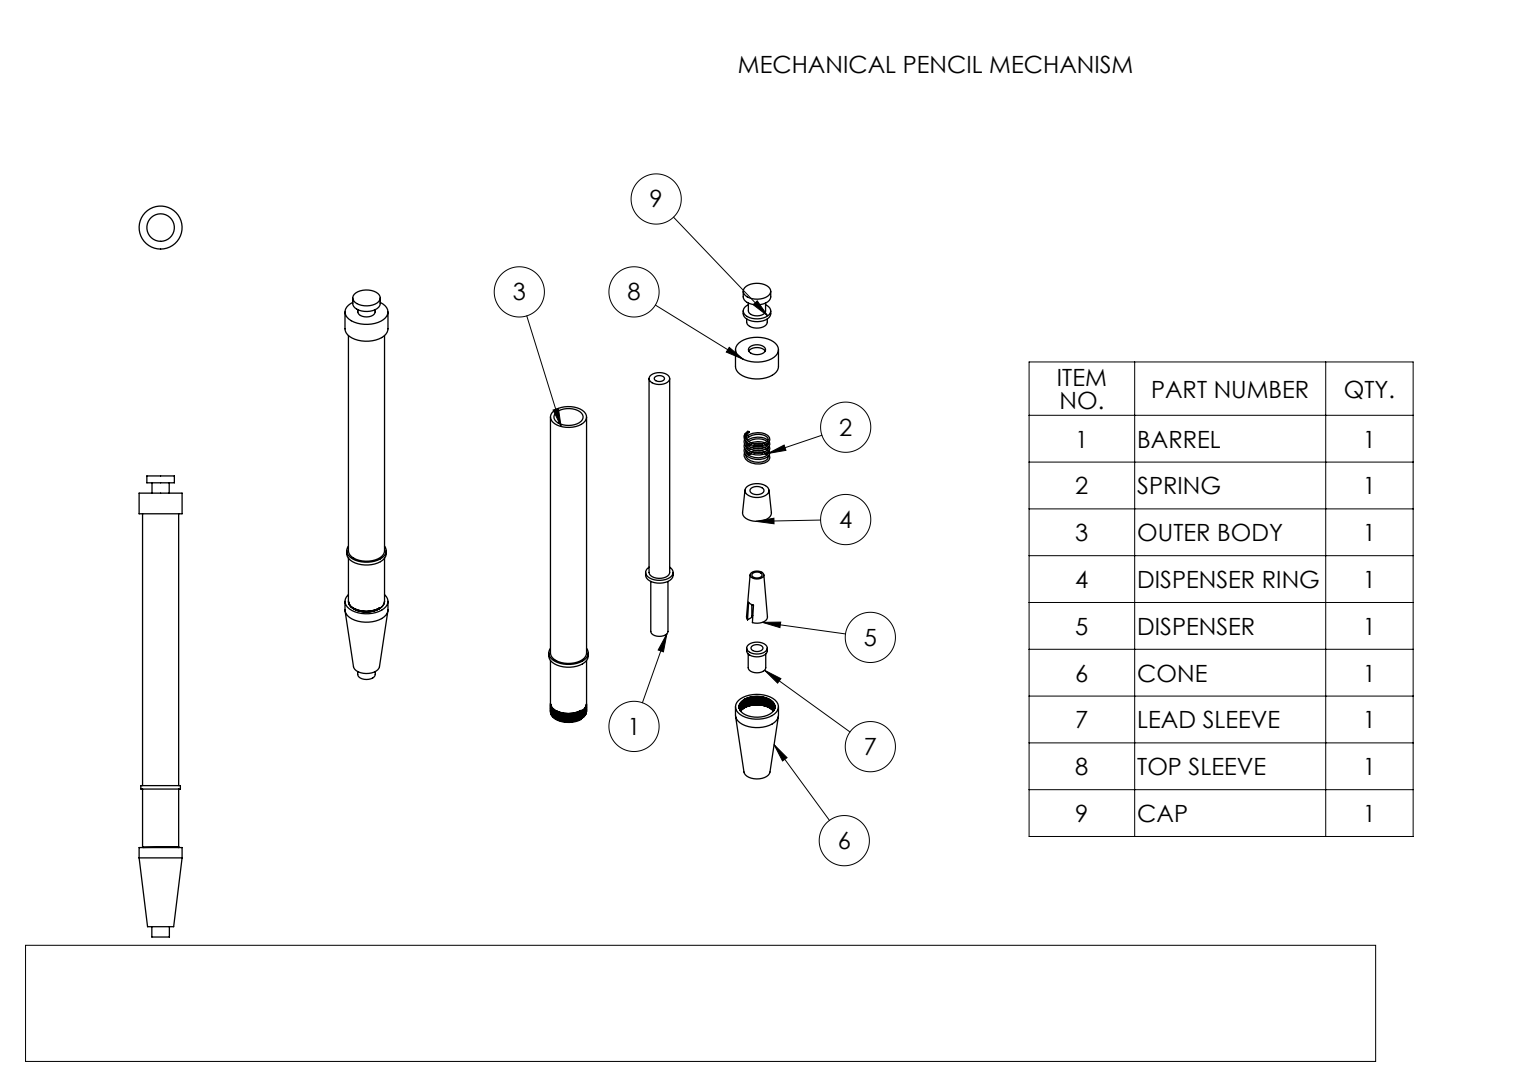
ISO-10303-21;
HEADER;
FILE_DESCRIPTION (('STEP AP214'),
    '1' );
FILE_NAME ('MAS-161',
    '2026-10-27T10:49:47',
    ( '' ),
    ( '' ),
    'SwSTEP 2.0',
    'SolidWorks 2026',
    '' );
FILE_SCHEMA (( 'AUTOMOTIVE_DESIGN' ));
ENDSEC;

DATA;
#1 = ORIENTED_EDGE ( 'NONE', *, *, #5722, .T. ) ;
#2 = FILL_AREA_STYLE ('',( #5004 ) ) ;
#3 = CARTESIAN_POINT ( 'NONE',  ( 1.113604000661152470E-15, -29.93749999999999645, 6.062177826491070398 ) ) ;
#4 = CARTESIAN_POINT ( 'NONE',  ( 5.114683531250000748, -27.33854166700806587, -2.952963913586932776 ) ) ;
#5 = CARTESIAN_POINT ( 'NONE',  ( -2.108492589042352261, -1.550659073900639395, 2.134148098076933397 ) ) ;
#6 = CARTESIAN_POINT ( 'NONE',  ( 5.250000000000000000, -29.22916666666666430, -3.031088913245534755 ) ) ;
#7 = CARTESIAN_POINT ( 'NONE',  ( 1.000000000000000000, -30.99987166532831395, 2.582963027349738816 ) ) ;
#8 = ADVANCED_FACE ( 'NONE', ( #6134 ), #1014, .T. ) ;
#9 = CARTESIAN_POINT ( 'NONE',  ( 5.114683531250000748, -28.90104166700806587, -2.952963913586932776 ) ) ;
#10 = VECTOR ( 'NONE', #8817, 1000.000000000000000 ) ;
#11 =( NAMED_UNIT ( * ) SI_UNIT ( $, .STERADIAN. ) SOLID_ANGLE_UNIT ( ) );
#12 = CARTESIAN_POINT ( 'NONE',  ( -5.114683531249999859, -28.31770833367473372, -2.952963913586935440 ) ) ;
#13 = CARTESIAN_POINT ( 'NONE',  ( 2.625000000000002220, -29.35416666598386826, 4.546633369868302132 ) ) ;
#14 = CARTESIAN_POINT ( 'NONE',  ( 5.249999999999999112, -27.54166666598387181, -3.031088913245536975 ) ) ;
#15 = CARTESIAN_POINT ( 'NONE',  ( -2.593667801677444817, -2.017599804162952387E-16, 2.576081167903025104 ) ) ;
#16 = DIRECTION ( 'NONE',  ( 1.000000000000000000, 0.000000000000000000, -0.000000000000000000 ) ) ;
#17 = CARTESIAN_POINT ( 'NONE',  ( -5.114683531249999859, -29.56770833367473017, -2.952963913586935440 ) ) ;
#18 = CARTESIAN_POINT ( 'NONE',  ( -1.467888652719046449, -6.949340926099361049, 3.492485675378536047 ) ) ;
#19 = EDGE_LOOP ( 'NONE', ( #3750, #4304, #1709, #1694 ) ) ;
#20 = CARTESIAN_POINT ( 'NONE',  ( -5.249999999999997335, -28.91666666598386826, 3.031088913245538308 ) ) ;
#21 = CARTESIAN_POINT ( 'NONE',  ( 2.557341765624996821, -29.15104166700806587, 4.429445870380401828 ) ) ;
#22 = EDGE_LOOP ( 'NONE', ( #1173, #7087 ) ) ;
#23 = ORIENTED_EDGE ( 'NONE', *, *, #2711, .F. ) ;
#24 = CARTESIAN_POINT ( 'NONE',  ( 0.000000000000000000, -53.00000000000000000, 0.000000000000000000 ) ) ;
#25 = CARTESIAN_POINT ( 'NONE',  ( 0.01814118441313990887, -6.550659073900639839, 3.500000000000000000 ) ) ;
#26 = CARTESIAN_POINT ( 'NONE',  ( 4.898587196589412829E-16, 81.00000000000001421, 4.000000000000000000 ) ) ;
#27 = VERTEX_POINT ( 'NONE', #2510 ) ;
#28 = PRODUCT_DEFINITION_SHAPE ( 'NONE', 'NONE',  #6653 ) ;
#29 = CARTESIAN_POINT ( 'NONE',  ( 6.429395695523604153E-16, -27.00000000000000000, 5.250000000000000000 ) ) ;
#30 = CARTESIAN_POINT ( 'NONE',  ( -1.000000000000000000, -29.00000000000000355, -1.118033988749894680 ) ) ;
#31 = CARTESIAN_POINT ( 'NONE',  ( 2.625000000000002220, -28.91666666666666785, 4.546633369868302132 ) ) ;
#32 = CARTESIAN_POINT ( 'NONE',  ( -5.114683531249999859, -28.75520833367473017, -2.952963913586935440 ) ) ;
#33 = CARTESIAN_POINT ( 'NONE',  ( 3.492485675378536047, -0.9493409260993610488, 1.467888652719046672 ) ) ;
#34 = CARTESIAN_POINT ( 'NONE',  ( -5.249999999999999112, -28.70833333265053611, -3.031088913245534755 ) ) ;
#35 = ADVANCED_FACE ( 'NONE', ( #4002 ), #1115, .T. ) ;
#36 = CARTESIAN_POINT ( 'NONE',  ( 1.260781871532495657, -2.949340926099361937, -2.992485675378538268 ) ) ;
#37 =( BOUNDED_CURVE ( )  B_SPLINE_CURVE ( 2, ( #980, #8007, #3923, #3739, #4569, #5213, #3046, #6700, #6561 ),
 .UNSPECIFIED., .F., .F. ) 
 B_SPLINE_CURVE_WITH_KNOTS ( ( 3, 2, 2, 2, 3 ),
 ( 0.1041666666666666713, 0.1111111111111111049, 0.1250000000000000000, 0.1388888888888888951, 0.1458333333333333426 ),
 .UNSPECIFIED. ) 
 CURVE ( )  GEOMETRIC_REPRESENTATION_ITEM ( )  RATIONAL_B_SPLINE_CURVE ( ( 0.9330127018922194093, 0.9330127018922194093, 1.000000000000000000, 0.8660254037844387076, 1.000000000000000000, 0.8660254037844387076, 1.000000000000000000, 0.9330127018922194093, 0.9330127018922194093 ) ) 
 REPRESENTATION_ITEM ( '' )  );
#38 = CARTESIAN_POINT ( 'NONE',  ( 1.406733260263403507, -28.57366454968462577, -5.249999999999994671 ) ) ;
#39 = CARTESIAN_POINT ( 'NONE',  ( 5.385316468750000141, -27.73437499965860198, -6.595110575850215044E-16 ) ) ;
#40 = CARTESIAN_POINT ( 'NONE',  ( 1.638713065079247855, -2.450659073900638862, -4.007514324621431534 ) ) ;
#41 = VECTOR ( 'NONE', #4397, 1000.000000000000000 ) ;
#42 = SURFACE_STYLE_FILL_AREA ( #6405 ) ;
#43 = APPLICATION_CONTEXT ( 'automotive_design' ) ;
#44 = CARTESIAN_POINT ( 'NONE',  ( 2.033577675846918216E-14, -27.81249999999999645, 5.250000000000000888 ) ) ;
#45 = ORIENTED_EDGE ( 'NONE', *, *, #6013, .T. ) ;
#46 = CARTESIAN_POINT ( 'NONE',  ( 5.385316468750000141, -27.45312499965860198, -6.595110575850215044E-16 ) ) ;
#47 =( GEOMETRIC_REPRESENTATION_CONTEXT ( 3 ) GLOBAL_UNCERTAINTY_ASSIGNED_CONTEXT ( ( #2399 ) ) GLOBAL_UNIT_ASSIGNED_CONTEXT ( ( #4022, #5674, #2943 ) ) REPRESENTATION_CONTEXT ( 'NONE', 'WORKASPACE' ) );
#48 = ORIENTED_EDGE ( 'NONE', *, *, #6878, .T. ) ;
#49 = CARTESIAN_POINT ( 'NONE',  ( -5.385316468750000141, -27.32812499965860198, 0.000000000000000000 ) ) ;
#50 = CARTESIAN_POINT ( 'NONE',  ( 2.992485675378565357, -0.6506590739006395951, -1.260781871532430376 ) ) ;
#51 = ORIENTED_EDGE ( 'NONE', *, *, #9169, .T. ) ;
#52 = CARTESIAN_POINT ( 'NONE',  ( -2.624999999999998668, -28.91666666666666785, -4.546633369868303021 ) ) ;
#53 = CYLINDRICAL_SURFACE ( 'NONE', #3617, 5.250000000000000000 ) ;
#54 = CIRCLE ( 'NONE', #4368, 3.000000000000000444 ) ;
#55 = CARTESIAN_POINT ( 'NONE',  ( 5.114683531250000748, -28.42187500034139802, 0.000000000000000000 ) ) ;
#56 = CARTESIAN_POINT ( 'NONE',  ( 3.616337804771879580E-16, -28.35937500034139447, -5.905927827173866440 ) ) ;
#57 = DIRECTION ( 'NONE',  ( 0.000000000000000000, 0.000000000000000000, -1.000000000000000000 ) ) ;
#58 = CARTESIAN_POINT ( 'NONE',  ( 2.324088772396477476E-15, -27.49999999931720751, -5.250000000000000000 ) ) ;
#59 = CARTESIAN_POINT ( 'NONE',  ( -2.110065146580993645, -1.191525181865938352E-11, 2.889420178070662093 ) ) ;
#60 = LINE ( 'NONE', #4208, #5677 ) ;
#61 = CARTESIAN_POINT ( 'NONE',  ( -1.431606283892620235, -7.949340926099361049, -3.507514324621463953 ) ) ;
#62 = CARTESIAN_POINT ( 'NONE',  ( -1.467888652719046449, -3.749340926099360871, 3.492485675378536047 ) ) ;
#63 = EDGE_LOOP ( 'NONE', ( #2688, #9138, #7959, #2580 ) ) ;
#64 = CARTESIAN_POINT ( 'NONE',  ( 2.161402558328724325E-14, -28.99999999931720751, -5.250000000000000000 ) ) ;
#65 = CARTESIAN_POINT ( 'NONE',  ( 5.250000000000000000, -27.03125000068279604, 0.000000000000000000 ) ) ;
#66 = EDGE_LOOP ( 'NONE', ( #5126, #5183, #1901, #2100 ) ) ;
#67 = ORIENTED_EDGE ( 'NONE', *, *, #7886, .F. ) ;
#68 = DIRECTION ( 'NONE',  ( 0.000000000000000000, -1.000000000000000000, 0.000000000000000000 ) ) ;
#69 = CARTESIAN_POINT ( 'NONE',  ( 2.487701488670203354, -6.750659073900639129, 2.462045979635629323 ) ) ;
#70 = CARTESIAN_POINT ( 'NONE',  ( 1.000000000000000000, -29.00000000000000355, -2.431755684948965435 ) ) ;
#71 = EDGE_LOOP ( 'NONE', ( #3557, #48, #247, #244 ) ) ;
#72 = DIRECTION ( 'NONE',  ( -0.000000000000000000, 1.000000000000000000, -0.000000000000000000 ) ) ;
#73 = CYLINDRICAL_SURFACE ( 'NONE', #5825, 2.499999999999999556 ) ;
#74 = EDGE_CURVE ( 'NONE', #2716, #8116, #2372, .T. ) ;
#75 = LINE ( 'NONE', #5700, #8771 ) ;
#76 = CARTESIAN_POINT ( 'NONE',  ( -2.557341765624999042, -27.02604166700806232, -4.429445870380400052 ) ) ;
#77 = CARTESIAN_POINT ( 'NONE',  ( -3.507514324621464397, -0.3493409260993610710, 1.431606283892619347 ) ) ;
#78 = CARTESIAN_POINT ( 'NONE',  ( -3.000000000000000444, -5.049340926099361582, -0.01814118441320822922 ) ) ;
#79 = EDGE_CURVE ( 'NONE', #7374, #1200, #6541, .T. ) ;
#80 = DIRECTION ( 'NONE',  ( 0.000000000000000000, 0.000000000000000000, -1.000000000000000000 ) ) ;
#81 = CARTESIAN_POINT ( 'NONE',  ( -3.807688866302469071E-16, -28.17187499965860553, -6.218427825808274356 ) ) ;
#82 = CARTESIAN_POINT ( 'NONE',  ( 0.01814118441321938349, -1.449340926099360827, -4.000000000000000000 ) ) ;
#83 = FACE_OUTER_BOUND ( 'NONE', #879, .T. ) ;
#84 = CARTESIAN_POINT ( 'NONE',  ( 0.000000000000000000, -30.00000000000000000, 0.000000000000000000 ) ) ;
#85 =( BOUNDED_CURVE ( )  B_SPLINE_CURVE ( 2, ( #9078, #8390, #6906, #2534, #530 ),
 .UNSPECIFIED., .F., .F. ) 
 B_SPLINE_CURVE_WITH_KNOTS ( ( 3, 2, 3 ),
 ( 0.9791666666666667407, 0.9861111111111111605, 1.000000000000000000 ),
 .UNSPECIFIED. ) 
 CURVE ( )  GEOMETRIC_REPRESENTATION_ITEM ( )  RATIONAL_B_SPLINE_CURVE ( ( 0.9330127018922192983, 0.9330127018922198534, 1.000000000000000000, 0.8660254037844387076, 1.000000000000000000 ) ) 
 REPRESENTATION_ITEM ( '' )  );
#86 = ORIENTED_EDGE ( 'NONE', *, *, #5112, .F. ) ;
#87 = CARTESIAN_POINT ( 'NONE',  ( -5.250000000000000000, -29.75000000000000000, 0.000000000000000000 ) ) ;
#88 = EDGE_LOOP ( 'NONE', ( #8020, #7590 ) ) ;
#89 = LINE ( 'NONE', #7305, #4201 ) ;
#90 = CARTESIAN_POINT ( 'NONE',  ( 2.134148098076933397, -5.150659073900639484, 2.108492589042352261 ) ) ;
#91 = ORIENTED_EDGE ( 'NONE', *, *, #709, .F. ) ;
#92 = CARTESIAN_POINT ( 'NONE',  ( -2.625000000000002220, -28.58333333333333215, 4.546633369868302132 ) ) ;
#93 = CYLINDRICAL_SURFACE ( 'NONE', #1391, 5.250000000000000000 ) ;
#94 = CARTESIAN_POINT ( 'NONE',  ( -5.114683531250000748, -28.06770833367473017, -2.952963913586935440 ) ) ;
#95 =( NAMED_UNIT ( * ) SI_UNIT ( $, .STERADIAN. ) SOLID_ANGLE_UNIT ( ) );
#96 = CARTESIAN_POINT ( 'NONE',  ( 5.114683531249998971, -27.44270833367473017, 2.952963913586936329 ) ) ;
#97 = EDGE_CURVE ( 'NONE', #451, #2823, #2727, .T. ) ;
#98 = CARTESIAN_POINT ( 'NONE',  ( 2.161402558328724325E-14, -28.74999999931720751, -5.250000000000000000 ) ) ;
#99 = PRODUCT_DEFINITION_SHAPE ( 'NONE', 'NONE',  #1543 ) ;
#100 = CARTESIAN_POINT ( 'NONE',  ( 0.000000000000000000, -30.00000000000000000, 4.250000000000000000 ) ) ;
#101 = DIRECTION ( 'NONE',  ( 0.000000000000000000, 1.000000000000000000, 0.000000000000000000 ) ) ;
#102 = CARTESIAN_POINT ( 'NONE',  ( -5.250000000000000888, -27.38541666734946389, 3.031088913245533423 ) ) ;
#103 = CARTESIAN_POINT ( 'NONE',  ( 3.616337804771879580E-16, -29.60937500034139447, -5.905927827173866440 ) ) ;
#104 = CARTESIAN_POINT ( 'NONE',  ( 3.492485675378536047, -7.349340926099362292, 1.467888652719046672 ) ) ;
#105 = VERTEX_POINT ( 'NONE', #315 ) ;
#106 = CARTESIAN_POINT ( 'NONE',  ( -6.972266317189433020E-16, -27.06250000000000000, -5.250000000000000000 ) ) ;
#107 = CARTESIAN_POINT ( 'NONE',  ( 0.000000000000000000, -29.00000000000000355, -1.499999999999999778 ) ) ;
#108 = CARTESIAN_POINT ( 'NONE',  ( -2.557341765624999042, -28.27604166700806587, -4.429445870380400052 ) ) ;
#109 = EDGE_LOOP ( 'NONE', ( #5447, #4357, #2145, #3993 ) ) ;
#110 =( BOUNDED_CURVE ( )  B_SPLINE_CURVE ( 2, ( #4913, #7058, #9104, #4136, #4827, #6270, #4182, #2042, #682 ),
 .UNSPECIFIED., .F., .T. ) 
 B_SPLINE_CURVE_WITH_KNOTS ( ( 3, 2, 2, 2, 3 ),
 ( 0.3541666666666666852, 0.3611111111111111049, 0.3750000000000000000, 0.3888888888888888951, 0.3958333333333333703 ),
 .UNSPECIFIED. ) 
 CURVE ( )  GEOMETRIC_REPRESENTATION_ITEM ( )  RATIONAL_B_SPLINE_CURVE ( ( 0.9330127018922194093, 0.9330127018922196314, 1.000000000000000000, 0.8660254037844387076, 1.000000000000000000, 0.8660254037844387076, 1.000000000000000000, 0.9330127018922190762, 0.9330127018922194093 ) ) 
 REPRESENTATION_ITEM ( '' )  );
#111 = ORIENTED_EDGE ( 'NONE', *, *, #9064, .F. ) ;
#112 = CARTESIAN_POINT ( 'NONE',  ( -2.033577675846918216E-14, -29.68750000000000355, 5.250000000000000888 ) ) ;
#113 = CARTESIAN_POINT ( 'NONE',  ( -5.385316468750001029, -27.13020833299193413, -3.109213912904136734 ) ) ;
#114 = CARTESIAN_POINT ( 'NONE',  ( -4.000000000000000000, -7.750659073900639129, 0.01814118441313491634 ) ) ;
#115 = CARTESIAN_POINT ( 'NONE',  ( 1.836970198721029688E-16, -29.00000000000000355, 1.499999999999999778 ) ) ;
#116 = VERTEX_POINT ( 'NONE', #4866 ) ;
#117 = DIRECTION ( 'NONE',  ( 0.000000000000000000, -0.000000000000000000, 1.000000000000000000 ) ) ;
#118 = CARTESIAN_POINT ( 'NONE',  ( 5.250000000000000000, -29.03125000068279604, 0.000000000000000000 ) ) ;
#119 = CARTESIAN_POINT ( 'NONE',  ( -2.033577675846918216E-14, -29.87499999931720396, 5.250000000000000888 ) ) ;
#120 = UNCERTAINTY_MEASURE_WITH_UNIT (LENGTH_MEASURE( 1.000000000000000082E-05 ), #327, 'distance_accuracy_value', 'NONE');
#121 = CARTESIAN_POINT ( 'NONE',  ( 2.557341765624996821, -27.15104166700806587, 4.429445870380401828 ) ) ;
#122 = CARTESIAN_POINT ( 'NONE',  ( -2.487701488670255312, -2.049340926099361582, 2.462045979635577808 ) ) ;
#123 = CIRCLE ( 'NONE', #1315, 2.629341307491595447 ) ;
#124 = CYLINDRICAL_SURFACE ( 'NONE', #4810, 5.250000000000000000 ) ;
#125 = CARTESIAN_POINT ( 'NONE',  ( 3.000000000000000444, -5.849340926099360516, 0.01814118441320859698 ) ) ;
#126 = LINE ( 'NONE', #643, #8886 ) ;
#127 = CARTESIAN_POINT ( 'NONE',  ( -1.674995433905599462, -0.5493409260993608045, 3.992485675378533383 ) ) ;
#128 = DIRECTION ( 'NONE',  ( 0.000000000000000000, 0.000000000000000000, 1.000000000000000000 ) ) ;
#129 = AXIS2_PLACEMENT_3D ( 'NONE', #454, #8273, #5425 ) ;
#130 = CARTESIAN_POINT ( 'NONE',  ( 0.000000000000000000, -9.999999999999998224, 0.000000000000000000 ) ) ;
#131 = ADVANCED_FACE ( 'NONE', ( #1342 ), #6353, .T. ) ;
#132 = ORIENTED_EDGE ( 'NONE', *, *, #6059, .F. ) ;
#133 = CARTESIAN_POINT ( 'NONE',  ( -5.385316468750000141, -28.82812499965860198, 0.000000000000000000 ) ) ;
#134 = FACE_OUTER_BOUND ( 'NONE', #6393, .T. ) ;
#135 = ORIENTED_EDGE ( 'NONE', *, *, #4743, .T. ) ;
#136 = AXIS2_PLACEMENT_3D ( 'NONE', #8169, #1046, #2544 ) ;
#137 = CARTESIAN_POINT ( 'NONE',  ( -2.692658234375000514, -27.61979166632526628, -4.663820869356205989 ) ) ;
#138 = CARTESIAN_POINT ( 'NONE',  ( 3.007514324621436863, -6.850659073900641438, 1.224499502706140719 ) ) ;
#139 = ORIENTED_EDGE ( 'NONE', *, *, #8501, .F. ) ;
#140 = CARTESIAN_POINT ( 'NONE',  ( 2.624999999999996891, -29.04166666666666785, 4.546633369868304797 ) ) ;
#141 = CARTESIAN_POINT ( 'NONE',  ( 2.624999999999996891, -29.79166666666666430, 4.546633369868304797 ) ) ;
#142 = PRESENTATION_LAYER_ASSIGNMENT (  '', '', ( #446 ) ) ;
#143 = CARTESIAN_POINT ( 'NONE',  ( 5.114683531250000748, -27.67187500034139802, 0.000000000000000000 ) ) ;
#144 = EDGE_CURVE ( 'NONE', #7348, #2527, #110, .T. ) ;
#145 =( LENGTH_UNIT ( ) NAMED_UNIT ( * ) SI_UNIT ( .MILLI., .METRE. ) );
#146 = CARTESIAN_POINT ( 'NONE',  ( 3.616337804771879580E-16, -27.35937500034140157, -5.905927827173866440 ) ) ;
#147 = AXIS2_PLACEMENT_3D ( 'NONE', #204, #847, #6661 ) ;
#148 = DIRECTION ( 'NONE',  ( 0.000000000000000000, 0.000000000000000000, 1.000000000000000000 ) ) ;
#149 = CARTESIAN_POINT ( 'NONE',  ( 1.431606283892619125, -5.549340926099361582, 3.507514324621464397 ) ) ;
#150 = FACE_OUTER_BOUND ( 'NONE', #5421, .T. ) ;
#151 = DIRECTION ( 'NONE',  ( 0.000000000000000000, -1.000000000000000000, 0.000000000000000000 ) ) ;
#152 = CARTESIAN_POINT ( 'NONE',  ( -1.467888652719046449, -6.949340926099361049, 3.492485675378536047 ) ) ;
#153 = DIRECTION ( 'NONE',  ( 1.000000000000000000, 0.000000000000000000, 0.000000000000000000 ) ) ;
#154 = VERTEX_POINT ( 'NONE', #6883 ) ;
#155 = CARTESIAN_POINT ( 'NONE',  ( 2.487701488670203354, -6.750659073900639129, 2.462045979635629323 ) ) ;
#156 = AXIS2_PLACEMENT_3D ( 'NONE', #2203, #2343, #5173 ) ;
#157 = CARTESIAN_POINT ( 'NONE',  ( 2.557341765624996821, -28.65104166700806587, 4.429445870380401828 ) ) ;
#158 = ORIENTED_EDGE ( 'NONE', *, *, #8454, .T. ) ;
#159 = DIRECTION ( 'NONE',  ( 0.000000000000000000, 0.000000000000000000, 1.000000000000000000 ) ) ;
#160 = CARTESIAN_POINT ( 'NONE',  ( 1.975475456537005874E-15, -29.62499999931719685, 5.249999999999999112 ) ) ;
#161 = CARTESIAN_POINT ( 'NONE',  ( -1.674995433905516196, -5.850659073900638774, -3.992485675378566690 ) ) ;
#162 = SURFACE_STYLE_USAGE ( .BOTH. , #5228 ) ;
#163 = ORIENTED_EDGE ( 'NONE', *, *, #1050, .T. ) ;
#164 = CARTESIAN_POINT ( 'NONE',  ( -2.625000000000000444, -27.97916666598386826, -4.546633369868303021 ) ) ;
#165 = CARTESIAN_POINT ( 'NONE',  ( 5.250000000000000000, -29.89062500034139802, 0.000000000000000000 ) ) ;
#166 =( BOUNDED_SURFACE ( )  B_SPLINE_SURFACE ( 1, 2, ( 
 ( #818, #6351, #7897, #2127, #6396, #4313, #4951, #7148, #3203, #6718, #3899, #5281, #6630, #911, #4591, #7235, #8126, #4545, #1608, #8029, #1563, #6587, #3708, #352, #8774, #6533, #1660, #1756, #258, #958, #3109, #3758, #6675, #8725, #7332, #4500, #215, #859, #1053, #7285, #3067, #3804, #3016, #5234, #5886, #5091, #4447, #167, #2357, #7377, #305, #5186, #5841, #6023, #5933, #2404, #8079, #8680, #1707, #1003, #7942, #3849, #2312, #3158, #5976, #8819, #2455, #2263, #5138, #7428, #4404, #7981, #4124, #8269, #545, #7618, #1856, #6123, #7569, #1243, #4085, #4819, #1104, #6920, #1900, #6958, #1989, #4775, #589, #3433, #1946, #3386, #1149, #4683, #3246, #6823, #6218, #8223, #2553, #7663, #8860, #9047, #5420, #6173, #4636, #5373, #7474, #7520, #2500, #399, #2692, #8952, #6772, #3992, #5323, #5519, #8364, #1285, #6070, #8177, #449, #1803, #3295, #6873, #3944, #4728, #1198, #499, #2603, #4041, #8906, #3344, #9000, #2647, #5469, #8315, #2033, #1328, #7703, #4856, #8406, #9093, #5561, #7005, #630 ),
 ( #2737, #6262, #4171, #7436, #8826, #964, #4457, #8135, #1571, #2461, #8086, #5147, #2366, #5099, #918, #7244, #1061, #3117, #868, #5196, #5286, #3811, #4510, #6636, #7294, #1010, #3073, #1667, #8038, #3905, #1713, #4552, #3768, #1618, #175, #6595, #7386, #7989, #8688, #1763, #6728, #3164, #7339, #5940, #4413, #2319, #3718, #225, #359, #6543, #3858, #5894, #3027, #8734, #2272, #4598, #5802, #8640, #5849, #6681, #265, #7949, #8782, #2411, #5242, #311, #5985, #6950, #6995, #2773, #3551, #4115, #2023, #5510, #3463, #579, #8353, #621, #750, #2861, #2724, #703, #4808, #4933, #3423, #5679, #6373, #1978, #4848, #6209, #7694, #4247, #7790, #7127, #5637, #6331, #2063, #2107, #8526, #2680, #9084, #8397, #9038, #6252, #13, #5593, #2816, #7654, #5551, #1277, #7039, #1318, #4891, #1408, #8486, #7743, #4162, #6292, #9128, #1447, #4291, #8437, #9167, #7081, #2155, #664, #1365, #4204, #3508, #4974, #7828, #5912, #4337, #7263, #4428, #797, #1687, #1544, #3641, #4527, #2335, #7172, #5215, #839, #7357 ) ),
 .UNSPECIFIED., .F., .F., .T. ) 
 B_SPLINE_SURFACE_WITH_KNOTS ( ( 2, 2 ),
 ( 3, 2, 2, 2, 2, 2, 2, 2, 2, 2, 2, 2, 2, 2, 2, 2, 2, 2, 2, 2, 2, 2, 2, 2, 2, 2, 2, 2, 2, 2, 2, 2, 2, 2, 2, 2, 2, 2, 2, 2, 2, 2, 2, 2, 2, 2, 2, 2, 2, 2, 2, 2, 2, 2, 2, 2, 2, 2, 2, 2, 2, 2, 2, 2, 2, 2, 2, 2, 2, 2, 2, 2, 3 ),
 ( 0.000000000000000000, 1.000000000000000000 ),
 ( 0.000000000000000000, 0.01388888888888888812, 0.02777777777777777624, 0.04166666666666666435, 0.05555555555555555247, 0.06944444444444444753, 0.08333333333333332871, 0.09722222222222222376, 0.1111111111111111049, 0.1250000000000000000, 0.1388888888888888951, 0.1527777777777777901, 0.1666666666666666574, 0.1805555555555555525, 0.1944444444444444475, 0.2083333333333333426, 0.2222222222222222099, 0.2361111111111111049, 0.2500000000000000000, 0.2638888888888888951, 0.2777777777777777901, 0.2916666666666666852, 0.3055555555555555802, 0.3194444444444444198, 0.3333333333333333148, 0.3472222222222222099, 0.3611111111111111049, 0.3750000000000000000, 0.3888888888888888951, 0.4027777777777777901, 0.4166666666666666852, 0.4305555555555555802, 0.4444444444444444198, 0.4583333333333333148, 0.4722222222222222099, 0.4861111111111111049, 0.5000000000000000000, 0.5138888888888888395, 0.5277777777777777901, 0.5416666666666666297, 0.5555555555555555802, 0.5694444444444444198, 0.5833333333333333703, 0.5972222222222222099, 0.6111111111111111605, 0.6250000000000000000, 0.6388888888888888395, 0.6527777777777777901, 0.6666666666666666297, 0.6805555555555555802, 0.6944444444444444198, 0.7083333333333333703, 0.7222222222222222099, 0.7361111111111111605, 0.7500000000000000000, 0.7638888888888888395, 0.7777777777777777901, 0.7916666666666666297, 0.8055555555555555802, 0.8194444444444444198, 0.8333333333333333703, 0.8472222222222222099, 0.8611111111111111605, 0.8750000000000000000, 0.8888888888888888395, 0.9027777777777777901, 0.9166666666666666297, 0.9305555555555555802, 0.9444444444444444198, 0.9583333333333333703, 0.9722222222222222099, 0.9861111111111111605, 1.000000000000000000 ),
 .UNSPECIFIED. ) 
 GEOMETRIC_REPRESENTATION_ITEM ( )  RATIONAL_B_SPLINE_SURFACE ( (
 ( 1.000000000000000000, 0.8660254037844387076, 1.000000000000000000, 0.8660254037844387076, 1.000000000000000000, 0.8660254037844387076, 1.000000000000000000, 0.8660254037844387076, 1.000000000000000000, 0.8660254037844387076, 1.000000000000000000, 0.8660254037844387076, 1.000000000000000000, 0.8660254037844387076, 1.000000000000000000, 0.8660254037844387076, 1.000000000000000000, 0.8660254037844387076, 1.000000000000000000, 0.8660254037844387076, 1.000000000000000000, 0.8660254037844387076, 1.000000000000000000, 0.8660254037844387076, 1.000000000000000000, 0.8660254037844387076, 1.000000000000000000, 0.8660254037844387076, 1.000000000000000000, 0.8660254037844387076, 1.000000000000000000, 0.8660254037844387076, 1.000000000000000000, 0.8660254037844387076, 1.000000000000000000, 0.8660254037844387076, 1.000000000000000000, 0.8660254037844387076, 1.000000000000000000, 0.8660254037844387076, 1.000000000000000000, 0.8660254037844387076, 1.000000000000000000, 0.8660254037844387076, 1.000000000000000000, 0.8660254037844387076, 1.000000000000000000, 0.8660254037844387076, 1.000000000000000000, 0.8660254037844387076, 1.000000000000000000, 0.8660254037844387076, 1.000000000000000000, 0.8660254037844387076, 1.000000000000000000, 0.8660254037844387076, 1.000000000000000000, 0.8660254037844387076, 1.000000000000000000, 0.8660254037844387076, 1.000000000000000000, 0.8660254037844387076, 1.000000000000000000, 0.8660254037844387076, 1.000000000000000000, 0.8660254037844387076, 1.000000000000000000, 0.8660254037844387076, 1.000000000000000000, 0.8660254037844387076, 1.000000000000000000, 0.8660254037844387076, 1.000000000000000000, 0.8660254037844387076, 1.000000000000000000, 0.8660254037844387076, 1.000000000000000000, 0.8660254037844387076, 1.000000000000000000, 0.8660254037844387076, 1.000000000000000000, 0.8660254037844387076, 1.000000000000000000, 0.8660254037844387076, 1.000000000000000000, 0.8660254037844387076, 1.000000000000000000, 0.8660254037844387076, 1.000000000000000000, 0.8660254037844387076, 1.000000000000000000, 0.8660254037844387076, 1.000000000000000000, 0.8660254037844387076, 1.000000000000000000, 0.8660254037844387076, 1.000000000000000000, 0.8660254037844387076, 1.000000000000000000, 0.8660254037844387076, 1.000000000000000000, 0.8660254037844387076, 1.000000000000000000, 0.8660254037844387076, 1.000000000000000000, 0.8660254037844387076, 1.000000000000000000, 0.8660254037844387076, 1.000000000000000000, 0.8660254037844387076, 1.000000000000000000, 0.8660254037844387076, 1.000000000000000000, 0.8660254037844387076, 1.000000000000000000, 0.8660254037844387076, 1.000000000000000000, 0.8660254037844387076, 1.000000000000000000, 0.8660254037844387076, 1.000000000000000000, 0.8660254037844387076, 1.000000000000000000, 0.8660254037844387076, 1.000000000000000000, 0.8660254037844387076, 1.000000000000000000, 0.8660254037844387076, 1.000000000000000000, 0.8660254037844387076, 1.000000000000000000, 0.8660254037844387076, 1.000000000000000000, 0.8660254037844387076, 1.000000000000000000, 0.8660254037844387076, 1.000000000000000000, 0.8660254037844387076, 1.000000000000000000, 0.8660254037844387076, 1.000000000000000000, 0.8660254037844387076, 1.000000000000000000, 0.8660254037844387076, 1.000000000000000000),
 ( 1.000000000000000000, 0.8660254037844387076, 1.000000000000000000, 0.8660254037844387076, 1.000000000000000000, 0.8660254037844387076, 1.000000000000000000, 0.8660254037844387076, 1.000000000000000000, 0.8660254037844387076, 1.000000000000000000, 0.8660254037844387076, 1.000000000000000000, 0.8660254037844387076, 1.000000000000000000, 0.8660254037844387076, 1.000000000000000000, 0.8660254037844387076, 1.000000000000000000, 0.8660254037844387076, 1.000000000000000000, 0.8660254037844387076, 1.000000000000000000, 0.8660254037844387076, 1.000000000000000000, 0.8660254037844387076, 1.000000000000000000, 0.8660254037844387076, 1.000000000000000000, 0.8660254037844387076, 1.000000000000000000, 0.8660254037844387076, 1.000000000000000000, 0.8660254037844387076, 1.000000000000000000, 0.8660254037844387076, 1.000000000000000000, 0.8660254037844387076, 1.000000000000000000, 0.8660254037844387076, 1.000000000000000000, 0.8660254037844387076, 1.000000000000000000, 0.8660254037844387076, 1.000000000000000000, 0.8660254037844387076, 1.000000000000000000, 0.8660254037844387076, 1.000000000000000000, 0.8660254037844387076, 1.000000000000000000, 0.8660254037844387076, 1.000000000000000000, 0.8660254037844387076, 1.000000000000000000, 0.8660254037844387076, 1.000000000000000000, 0.8660254037844387076, 1.000000000000000000, 0.8660254037844387076, 1.000000000000000000, 0.8660254037844387076, 1.000000000000000000, 0.8660254037844387076, 1.000000000000000000, 0.8660254037844387076, 1.000000000000000000, 0.8660254037844387076, 1.000000000000000000, 0.8660254037844387076, 1.000000000000000000, 0.8660254037844387076, 1.000000000000000000, 0.8660254037844387076, 1.000000000000000000, 0.8660254037844387076, 1.000000000000000000, 0.8660254037844387076, 1.000000000000000000, 0.8660254037844387076, 1.000000000000000000, 0.8660254037844387076, 1.000000000000000000, 0.8660254037844387076, 1.000000000000000000, 0.8660254037844387076, 1.000000000000000000, 0.8660254037844387076, 1.000000000000000000, 0.8660254037844387076, 1.000000000000000000, 0.8660254037844387076, 1.000000000000000000, 0.8660254037844387076, 1.000000000000000000, 0.8660254037844387076, 1.000000000000000000, 0.8660254037844387076, 1.000000000000000000, 0.8660254037844387076, 1.000000000000000000, 0.8660254037844387076, 1.000000000000000000, 0.8660254037844387076, 1.000000000000000000, 0.8660254037844387076, 1.000000000000000000, 0.8660254037844387076, 1.000000000000000000, 0.8660254037844387076, 1.000000000000000000, 0.8660254037844387076, 1.000000000000000000, 0.8660254037844387076, 1.000000000000000000, 0.8660254037844387076, 1.000000000000000000, 0.8660254037844387076, 1.000000000000000000, 0.8660254037844387076, 1.000000000000000000, 0.8660254037844387076, 1.000000000000000000, 0.8660254037844387076, 1.000000000000000000, 0.8660254037844387076, 1.000000000000000000, 0.8660254037844387076, 1.000000000000000000, 0.8660254037844387076, 1.000000000000000000, 0.8660254037844387076, 1.000000000000000000, 0.8660254037844387076, 1.000000000000000000, 0.8660254037844387076, 1.000000000000000000, 0.8660254037844387076, 1.000000000000000000, 0.8660254037844387076, 1.000000000000000000, 0.8660254037844387076, 1.000000000000000000, 0.8660254037844387076, 1.000000000000000000) ) ) 
 REPRESENTATION_ITEM ( '' )  SURFACE ( )  );
#167 = CARTESIAN_POINT ( 'NONE',  ( -5.385316468749998364, -28.08854166632526628, 3.109213912904140287 ) ) ;
#168 = CARTESIAN_POINT ( 'NONE',  ( 2.557341765625000818, -27.56770833367473017, -4.429445870380400052 ) ) ;
#169 = CARTESIAN_POINT ( 'NONE',  ( 2.462045979635577364, -2.449340926099361049, 2.487701488670255312 ) ) ;
#170 = CARTESIAN_POINT ( 'NONE',  ( 1.142306659890740623E-15, -27.26562499965860553, 6.218427825808274356 ) ) ;
#171 = CARTESIAN_POINT ( 'NONE',  ( 1.224499502706142273, -2.450659073900639751, -3.007514324621435531 ) ) ;
#172 = CARTESIAN_POINT ( 'NONE',  ( -5.249999999999997335, -29.41666666598387181, 3.031088913245538308 ) ) ;
#173 = EDGE_CURVE ( 'NONE', #105, #7348, #3624, .T. ) ;
#174 = CARTESIAN_POINT ( 'NONE',  ( -2.815599370228846876, -1.649340926099360560, -2.841254879263533262 ) ) ;
#175 = CARTESIAN_POINT ( 'NONE',  ( -2.624999999999996891, -27.89583333265053255, 4.546633369868304797 ) ) ;
#176 = LINE ( 'NONE', #7340, #7480 ) ;
#177 = CARTESIAN_POINT ( 'NONE',  ( 2.462045979635577364, -0.8493409260993610710, 2.487701488670255312 ) ) ;
#178 = DIRECTION ( 'NONE',  ( 0.000000000000000000, -1.000000000000000000, 0.000000000000000000 ) ) ;
#179 = VERTEX_POINT ( 'NONE', #5659 ) ;
#180 = CARTESIAN_POINT ( 'NONE',  ( 1.142306659890740623E-15, -27.76562499965860198, 6.218427825808274356 ) ) ;
#181 = CARTESIAN_POINT ( 'NONE',  ( -1.674995433905599462, -5.349340926099361404, 3.992485675378533383 ) ) ;
#182 = LINE ( 'NONE', #6689, #6964 ) ;
#183 = VERTEX_POINT ( 'NONE', #6311 ) ;
#184 = CARTESIAN_POINT ( 'NONE',  ( 2.692658234375002735, -27.24479166632526628, 4.663820869356205101 ) ) ;
#185 = CARTESIAN_POINT ( 'NONE',  ( 2.992485675378565357, -5.450659073900638418, -1.260781871532430376 ) ) ;
#186 = VECTOR ( 'NONE', #298, 1000.000000000000000 ) ;
#187 = VERTEX_POINT ( 'NONE', #5479 ) ;
#188 = CARTESIAN_POINT ( 'NONE',  ( -5.250000000000000000, -27.62500000000000000, -6.429395695523604153E-16 ) ) ;
#189 = CARTESIAN_POINT ( 'NONE',  ( 3.616337804771879580E-16, -28.35937500034139447, -5.905927827173866440 ) ) ;
#190 = AXIS2_PLACEMENT_3D ( 'NONE', #7645, #6857, #8348 ) ;
#191 = EDGE_CURVE ( 'NONE', #7471, #2074, #636, .T. ) ;
#192 = CARTESIAN_POINT ( 'NONE',  ( 2.557341765624996821, -26.96354166700806232, 4.429445870380401828 ) ) ;
#193 = CARTESIAN_POINT ( 'NONE',  ( -1.084901341431563726E-15, -29.67187500034139802, 5.905927827173866440 ) ) ;
#194 = ADVANCED_FACE ( 'NONE', ( #7672 ), #8416, .F. ) ;
#195 = CARTESIAN_POINT ( 'NONE',  ( 1.467888652719048226, -1.349340926099361182, -3.492485675378536047 ) ) ;
#196 = CARTESIAN_POINT ( 'NONE',  ( 7.654042494670957606E-16, -27.00000000000000000, 6.250000000000000000 ) ) ;
#197 = VECTOR ( 'NONE', #5888, 1000.000000000000000 ) ;
#198 = CARTESIAN_POINT ( 'NONE',  ( 0.000000000000000000, -50.00000000000000000, 0.000000000000000000 ) ) ;
#199 = CARTESIAN_POINT ( 'NONE',  ( 5.114683531250000748, -29.67187500034139802, 0.000000000000000000 ) ) ;
#200 = CARTESIAN_POINT ( 'NONE',  ( 2.624999999999996891, -27.32291666734946389, 4.546633369868304797 ) ) ;
#201 = VECTOR ( 'NONE', #4183, 1000.000000000000000 ) ;
#202 = ORIENTED_EDGE ( 'NONE', *, *, #7606, .T. ) ;
#203 = CARTESIAN_POINT ( 'NONE',  ( 3.507514324621434199, -6.850659073900639662, 1.431606283892693066 ) ) ;
#204 = CARTESIAN_POINT ( 'NONE',  ( 0.000000000000000000, 74.00000000000001421, 0.000000000000000000 ) ) ;
#205 = CARTESIAN_POINT ( 'NONE',  ( 3.616337804771879580E-16, -28.04687500034139802, -5.905927827173866440 ) ) ;
#206 = ADVANCED_FACE ( 'NONE', ( #2793 ), #8063, .F. ) ;
#207 = AXIS2_PLACEMENT_3D ( 'NONE', #5032, #1556, #5225 ) ;
#208 = ORIENTED_EDGE ( 'NONE', *, *, #3669, .T. ) ;
#209 = DIRECTION ( 'NONE',  ( 0.000000000000000000, -1.000000000000000000, 0.000000000000000000 ) ) ;
#210 = CARTESIAN_POINT ( 'NONE',  ( -5.385316468750001029, -27.88020833299193413, -3.109213912904136734 ) ) ;
#211 = CARTESIAN_POINT ( 'NONE',  ( -3.992485675378568022, -3.050659073900638951, 1.674995433905515529 ) ) ;
#212 = EDGE_LOOP ( 'NONE', ( #4167, #4581 ) ) ;
#213 = DIRECTION ( 'NONE',  ( 0.000000000000000000, 1.000000000000000000, 0.000000000000000000 ) ) ;
#214 = CARTESIAN_POINT ( 'NONE',  ( -1.113604000661152470E-15, -29.09375000068279249, 6.062177826491070398 ) ) ;
#215 = CARTESIAN_POINT ( 'NONE',  ( -5.385316468750000141, -27.85937499965860198, 0.000000000000000000 ) ) ;
#216 = CARTESIAN_POINT ( 'NONE',  ( -5.114683531249999859, -27.50520833367472662, -2.952963913586935440 ) ) ;
#217 = CARTESIAN_POINT ( 'NONE',  ( 0.000000000000000000, -9.000000000000000000, 0.000000000000000000 ) ) ;
#218 = FACE_OUTER_BOUND ( 'NONE', #2298, .T. ) ;
#219 = CARTESIAN_POINT ( 'NONE',  ( -3.000000000000000444, 0.2493409260993606213, 0.01814118441314532468 ) ) ;
#220 = PRODUCT_DEFINITION_CONTEXT ( 'detailed design', #4323, 'design' ) ;
#221 = DIRECTION ( 'NONE',  ( 0.000000000000000000, -1.000000000000000000, 0.000000000000000000 ) ) ;
#222 = EDGE_CURVE ( 'NONE', #8837, #8220, #2702, .T. ) ;
#223 = CARTESIAN_POINT ( 'NONE',  ( 1.674995433905601239, -1.349340926099360960, -3.992485675378532939 ) ) ;
#224 =( BOUNDED_SURFACE ( )  B_SPLINE_SURFACE ( 3, 2, ( 
 ( #862, #77, #7899, #2314, #3760, #7195, #3662, #33, #7151, #5702, #1518, #3711, #8682, #6487, #6589, #4994, #6536, #6398, #122, #8546, #2971, #5140, #169, #8636, #2266, #7944, #7851, #1565, #2618, #4787, #7676, #3958, #2660, #1914, #3403, #6785, #1117, #8281, #411, #1259, #1961, #1297, #6886, #559, #1872, #4052, #7630, #1212, #2704, #4098, #3259, #6231, #4005, #5387, #4739, #8237, #4140, #6931, #8418, #6085, #9063, #514, #3357, #3307, #3445, #7586, #5533, #6973, #6187, #6138, #8968, #5435, #5573, #8377, #463, #9015, #5482, #2004, #2569, #8330, #8920 ),
 ( #4830, #602, #6272, #4650, #9107, #2752, #7491, #4695, #1161, #7533, #6839, #4365, #5615, #2973, #6489, #3664, #5046, #6401, #684, #1520, #8590, #7198, #3576, #7811, #8508, #728, #7153, #36, #6809, #2176, #7901, #1345, #2887, #2133, #776, #4184, #7718, #5662, #7016, #7853, #8548, #822, #4269, #3622, #8463, #1428, #4996, #7105, #78, #1474, #642, #6445, #1385, #2796, #4956, #2091, #125, #4317, #5798, #3488, #2929, #5703, #5749, #3531, #2045, #2220, #4870, #6313, #9149, #6355, #2842, #4915, #7763, #4230, #7061, #6591, #5191, #5981, #6538, #4451, #7946 ),
 ( #219, #3207, #5284, #5143, #7290, #3762, #8823, #7381, #8131, #2459, #1568, #915, #8637, #3071, #6680, #1007, #355, #8084, #8778, #4505, #5890, #3856, #3021, #7433, #3902, #5845, #1059, #171, #864, #3808, #4549, #6723, #4409, #8684, #309, #2408, #3161, #1711, #7336, #2268, #2316, #8730, #5096, #7239, #4595, #2362, #8033, #1664, #962, #7985, #6634, #262, #3713, #1613, #1759, #3115, #5938, #5238, #3250, #4128, #3995, #6073, #6962, #4779, #402, #7666, #3299, #593, #4088, #3948, #6026, #2695, #2557, #4686, #1152, #3392, #7621, #5522, #6221, #5327, #1861 ),
 ( #1248, #8863, #5472, #6177, #1903, #7523, #6923, #8910, #4822, #1288, #5377, #2503, #6775, #7478, #1202, #1949, #8180, #1809, #8228, #549, #9004, #9051, #8319, #4731, #4640, #6828, #6126, #1108, #453, #1994, #8957, #2608, #5424, #8272, #7573, #4044, #6876, #504, #3347, #8368, #2650, #7093, #4259, #633, #1510, #1376, #3477, #4354, #2166, #7008, #5034, #675, #7189, #1460, #1332, #8539, #1419, #4219, #3565, #6434, #2744, #717, #3519, #4986, #5564, #9096, #7051, #8409, #25, #6389, #69, #5650, #7843, #6304, #2831, #2873, #9179, #4307, #5694, #2036, #7143 ),
 ( #4174, #766, #6345, #9141, #2785, #4859, #2920, #5737, #8498, #4903, #7891, #3608, #8582, #2210, #3436, #5605, #8450, #2077, #7754, #2120, #4946, #7707, #6265, #7802, #995, #5083, #6479, #6578, #8767, #952, #7371, #299, #2350, #211, #7279, #8718, #6624, #4494, #3153, #251, #5180, #1601, #4584, #5971, #3061, #8022, #2307, #5227, #906, #5881, #1654, #8675, #5785, #3102, #5129, #5835, #3842, #6668, #7325, #3801, #7937, #161, #1558, #7976, #5927, #8071, #3753, #8812, #7228, #2398, #811, #4442, #5275, #1701, #4538, #2449, #3011, #8119, #1748, #3654, #114 ),
 ( #2963, #8627, #2258, #4398, #855, #3702, #6527, #343, #1045, #3893, #6713, #3196, #7421, #4559, #1017, #7998, #366, #6735, #2514, #230, #1069, #8740, #877, #7444, #8143, #1625, #3171, #7346, #5154, #6601, #3727, #3911, #3215, #8045, #2374, #8873, #2468, #7394, #6688, #8094, #3079, #5901, #925, #3774, #3818, #5203, #6551, #6035, #1673, #5340, #2326, #181, #6643, #5993, #3865, #1722, #4516, #8189, #1818, #7251, #3035, #5292, #972, #272, #318, #5855, #4464, #8695, #7302, #3125, #5949, #2419, #8788, #5249, #8832, #1770, #4605, #1982, #8994, #8441, #625 ),
 ( #1940, #4813, #4769, #667, #3467, #4937, #6868, #6296, #6256, #3427, #9042, #9172, #1280, #5597, #3512, #7658, #2684, #5514, #4119, #2112, #7697, #6213, #8357, #6953, #7745, #8309, #583, #492, #9088, #7613, #3339, #2729, #1190, #7043, #6915, #5556, #8400, #1369, #9132, #6335, #4209, #6168, #2028, #4034, #4851, #2066, #2776, #2642, #4894, #1322, #4165, #6999, #2820, #1237, #5640, #8490, #4079, #5463, #539, #3380, #2954, #3690, #3052, #707, #4978, #6515, #1548, #152, #7218, #3645, #7795, #2158, #7879, #5869, #8709, #3745, #5727, #61, #5022, #2910, #8530 ) ),
 .UNSPECIFIED., .T., .F., .T. ) 
 B_SPLINE_SURFACE_WITH_KNOTS ( ( 4, 3, 4 ),
 ( 3, 2, 2, 2, 2, 2, 2, 2, 2, 2, 2, 2, 2, 2, 2, 2, 2, 2, 2, 2, 2, 2, 2, 2, 2, 2, 2, 2, 2, 2, 2, 2, 2, 2, 2, 2, 2, 2, 2, 2, 3 ),
 ( 0.000000000000000000, 0.5000000000000000000, 1.000000000000000000 ),
 ( 0.000000000000000000, 0.02500000000000000139, 0.05000000000000000278, 0.07499999999999999722, 0.1000000000000000056, 0.1250000000000000000, 0.1499999999999999944, 0.1749999999999999889, 0.2000000000000000111, 0.2250000000000000056, 0.2500000000000000000, 0.2750000000000000222, 0.2999999999999999889, 0.3250000000000000111, 0.3499999999999999778, 0.3750000000000000000, 0.4000000000000000222, 0.4249999999999999889, 0.4500000000000000111, 0.4749999999999999778, 0.5000000000000000000, 0.5250000000000000222, 0.5500000000000000444, 0.5749999999999999556, 0.5999999999999999778, 0.6250000000000000000, 0.6500000000000000222, 0.6750000000000000444, 0.6999999999999999556, 0.7249999999999999778, 0.7500000000000000000, 0.7750000000000000222, 0.8000000000000000444, 0.8249999999999999556, 0.8499999999999999778, 0.8750000000000000000, 0.9000000000000000222, 0.9250000000000000444, 0.9499999999999999556, 0.9749999999999999778, 1.000000000000000000 ),
 .UNSPECIFIED. ) 
 GEOMETRIC_REPRESENTATION_ITEM ( )  RATIONAL_B_SPLINE_SURFACE ( (
 ( 1.000000000000000000, 0.9238795325112867385, 1.000000000000000000, 0.9238795325112867385, 1.000000000000000000, 0.9238795325112867385, 1.000000000000000000, 0.9238795325112867385, 1.000000000000000000, 0.9238795325112867385, 1.000000000000000000, 0.9238795325112867385, 1.000000000000000000, 0.9238795325112867385, 1.000000000000000000, 0.9238795325112867385, 1.000000000000000000, 0.9238795325112867385, 1.000000000000000000, 0.9238795325112867385, 1.000000000000000000, 0.9238795325112867385, 1.000000000000000000, 0.9238795325112867385, 1.000000000000000000, 0.9238795325112867385, 1.000000000000000000, 0.9238795325112867385, 1.000000000000000000, 0.9238795325112867385, 1.000000000000000000, 0.9238795325112867385, 1.000000000000000000, 0.9238795325112867385, 1.000000000000000000, 0.9238795325112867385, 1.000000000000000000, 0.9238795325112867385, 1.000000000000000000, 0.9238795325112867385, 1.000000000000000000, 0.9238795325112867385, 1.000000000000000000, 0.9238795325112867385, 1.000000000000000000, 0.9238795325112867385, 1.000000000000000000, 0.9238795325112867385, 1.000000000000000000, 0.9238795325112867385, 1.000000000000000000, 0.9238795325112867385, 1.000000000000000000, 0.9238795325112867385, 1.000000000000000000, 0.9238795325112867385, 1.000000000000000000, 0.9238795325112867385, 1.000000000000000000, 0.9238795325112867385, 1.000000000000000000, 0.9238795325112867385, 1.000000000000000000, 0.9238795325112867385, 1.000000000000000000, 0.9238795325112867385, 1.000000000000000000, 0.9238795325112867385, 1.000000000000000000, 0.9238795325112867385, 1.000000000000000000, 0.9238795325112867385, 1.000000000000000000, 0.9238795325112867385, 1.000000000000000000, 0.9238795325112867385, 1.000000000000000000, 0.9238795325112867385, 1.000000000000000000, 0.9238795325112867385, 1.000000000000000000),
 ( 0.3333333333333333703, 0.3079598441704289313, 0.3333333333333333703, 0.3079598441704289313, 0.3333333333333333703, 0.3079598441704289313, 0.3333333333333333703, 0.3079598441704289313, 0.3333333333333333703, 0.3079598441704289313, 0.3333333333333333703, 0.3079598441704289313, 0.3333333333333333703, 0.3079598441704289313, 0.3333333333333333703, 0.3079598441704289313, 0.3333333333333333703, 0.3079598441704289313, 0.3333333333333333703, 0.3079598441704289313, 0.3333333333333333703, 0.3079598441704289313, 0.3333333333333333703, 0.3079598441704289313, 0.3333333333333333703, 0.3079598441704289313, 0.3333333333333333703, 0.3079598441704289313, 0.3333333333333333703, 0.3079598441704289313, 0.3333333333333333703, 0.3079598441704289313, 0.3333333333333333703, 0.3079598441704289313, 0.3333333333333333703, 0.3079598441704289313, 0.3333333333333333703, 0.3079598441704289313, 0.3333333333333333703, 0.3079598441704289313, 0.3333333333333333703, 0.3079598441704289313, 0.3333333333333333703, 0.3079598441704289313, 0.3333333333333333703, 0.3079598441704289313, 0.3333333333333333703, 0.3079598441704289313, 0.3333333333333333703, 0.3079598441704289313, 0.3333333333333333703, 0.3079598441704289313, 0.3333333333333333703, 0.3079598441704289313, 0.3333333333333333703, 0.3079598441704289313, 0.3333333333333333703, 0.3079598441704289313, 0.3333333333333333703, 0.3079598441704289313, 0.3333333333333333703, 0.3079598441704289313, 0.3333333333333333703, 0.3079598441704289313, 0.3333333333333333703, 0.3079598441704289313, 0.3333333333333333703, 0.3079598441704289313, 0.3333333333333333703, 0.3079598441704289313, 0.3333333333333333703, 0.3079598441704289313, 0.3333333333333333703, 0.3079598441704289313, 0.3333333333333333703, 0.3079598441704289313, 0.3333333333333333703, 0.3079598441704289313, 0.3333333333333333703, 0.3079598441704289313, 0.3333333333333333703),
 ( 0.3333333333333333703, 0.3079598441704289313, 0.3333333333333333703, 0.3079598441704289313, 0.3333333333333333703, 0.3079598441704289313, 0.3333333333333333703, 0.3079598441704289313, 0.3333333333333333703, 0.3079598441704289313, 0.3333333333333333703, 0.3079598441704289313, 0.3333333333333333703, 0.3079598441704289313, 0.3333333333333333703, 0.3079598441704289313, 0.3333333333333333703, 0.3079598441704289313, 0.3333333333333333703, 0.3079598441704289313, 0.3333333333333333703, 0.3079598441704289313, 0.3333333333333333703, 0.3079598441704289313, 0.3333333333333333703, 0.3079598441704289313, 0.3333333333333333703, 0.3079598441704289313, 0.3333333333333333703, 0.3079598441704289313, 0.3333333333333333703, 0.3079598441704289313, 0.3333333333333333703, 0.3079598441704289313, 0.3333333333333333703, 0.3079598441704289313, 0.3333333333333333703, 0.3079598441704289313, 0.3333333333333333703, 0.3079598441704289313, 0.3333333333333333703, 0.3079598441704289313, 0.3333333333333333703, 0.3079598441704289313, 0.3333333333333333703, 0.3079598441704289313, 0.3333333333333333703, 0.3079598441704289313, 0.3333333333333333703, 0.3079598441704289313, 0.3333333333333333703, 0.3079598441704289313, 0.3333333333333333703, 0.3079598441704289313, 0.3333333333333333703, 0.3079598441704289313, 0.3333333333333333703, 0.3079598441704289313, 0.3333333333333333703, 0.3079598441704289313, 0.3333333333333333703, 0.3079598441704289313, 0.3333333333333333703, 0.3079598441704289313, 0.3333333333333333703, 0.3079598441704289313, 0.3333333333333333703, 0.3079598441704289313, 0.3333333333333333703, 0.3079598441704289313, 0.3333333333333333703, 0.3079598441704289313, 0.3333333333333333703, 0.3079598441704289313, 0.3333333333333333703, 0.3079598441704289313, 0.3333333333333333703, 0.3079598441704289313, 0.3333333333333333703, 0.3079598441704289313, 0.3333333333333333703),
 ( 1.000000000000000000, 0.9238795325112867385, 1.000000000000000000, 0.9238795325112867385, 1.000000000000000000, 0.9238795325112867385, 1.000000000000000000, 0.9238795325112867385, 1.000000000000000000, 0.9238795325112867385, 1.000000000000000000, 0.9238795325112867385, 1.000000000000000000, 0.9238795325112867385, 1.000000000000000000, 0.9238795325112867385, 1.000000000000000000, 0.9238795325112867385, 1.000000000000000000, 0.9238795325112867385, 1.000000000000000000, 0.9238795325112867385, 1.000000000000000000, 0.9238795325112867385, 1.000000000000000000, 0.9238795325112867385, 1.000000000000000000, 0.9238795325112867385, 1.000000000000000000, 0.9238795325112867385, 1.000000000000000000, 0.9238795325112867385, 1.000000000000000000, 0.9238795325112867385, 1.000000000000000000, 0.9238795325112867385, 1.000000000000000000, 0.9238795325112867385, 1.000000000000000000, 0.9238795325112867385, 1.000000000000000000, 0.9238795325112867385, 1.000000000000000000, 0.9238795325112867385, 1.000000000000000000, 0.9238795325112867385, 1.000000000000000000, 0.9238795325112867385, 1.000000000000000000, 0.9238795325112867385, 1.000000000000000000, 0.9238795325112867385, 1.000000000000000000, 0.9238795325112867385, 1.000000000000000000, 0.9238795325112867385, 1.000000000000000000, 0.9238795325112867385, 1.000000000000000000, 0.9238795325112867385, 1.000000000000000000, 0.9238795325112867385, 1.000000000000000000, 0.9238795325112867385, 1.000000000000000000, 0.9238795325112867385, 1.000000000000000000, 0.9238795325112867385, 1.000000000000000000, 0.9238795325112867385, 1.000000000000000000, 0.9238795325112867385, 1.000000000000000000, 0.9238795325112867385, 1.000000000000000000, 0.9238795325112867385, 1.000000000000000000, 0.9238795325112867385, 1.000000000000000000, 0.9238795325112867385, 1.000000000000000000),
 ( 0.3333333333333333703, 0.3079598441704289313, 0.3333333333333333703, 0.3079598441704289313, 0.3333333333333333703, 0.3079598441704289313, 0.3333333333333333703, 0.3079598441704289313, 0.3333333333333333703, 0.3079598441704289313, 0.3333333333333333703, 0.3079598441704289313, 0.3333333333333333703, 0.3079598441704289313, 0.3333333333333333703, 0.3079598441704289313, 0.3333333333333333703, 0.3079598441704289313, 0.3333333333333333703, 0.3079598441704289313, 0.3333333333333333703, 0.3079598441704289313, 0.3333333333333333703, 0.3079598441704289313, 0.3333333333333333703, 0.3079598441704289313, 0.3333333333333333703, 0.3079598441704289313, 0.3333333333333333703, 0.3079598441704289313, 0.3333333333333333703, 0.3079598441704289313, 0.3333333333333333703, 0.3079598441704289313, 0.3333333333333333703, 0.3079598441704289313, 0.3333333333333333703, 0.3079598441704289313, 0.3333333333333333703, 0.3079598441704289313, 0.3333333333333333703, 0.3079598441704289313, 0.3333333333333333703, 0.3079598441704289313, 0.3333333333333333703, 0.3079598441704289313, 0.3333333333333333703, 0.3079598441704289313, 0.3333333333333333703, 0.3079598441704289313, 0.3333333333333333703, 0.3079598441704289313, 0.3333333333333333703, 0.3079598441704289313, 0.3333333333333333703, 0.3079598441704289313, 0.3333333333333333703, 0.3079598441704289313, 0.3333333333333333703, 0.3079598441704289313, 0.3333333333333333703, 0.3079598441704289313, 0.3333333333333333703, 0.3079598441704289313, 0.3333333333333333703, 0.3079598441704289313, 0.3333333333333333703, 0.3079598441704289313, 0.3333333333333333703, 0.3079598441704289313, 0.3333333333333333703, 0.3079598441704289313, 0.3333333333333333703, 0.3079598441704289313, 0.3333333333333333703, 0.3079598441704289313, 0.3333333333333333703, 0.3079598441704289313, 0.3333333333333333703, 0.3079598441704289313, 0.3333333333333333703),
 ( 0.3333333333333333703, 0.3079598441704289313, 0.3333333333333333703, 0.3079598441704289313, 0.3333333333333333703, 0.3079598441704289313, 0.3333333333333333703, 0.3079598441704289313, 0.3333333333333333703, 0.3079598441704289313, 0.3333333333333333703, 0.3079598441704289313, 0.3333333333333333703, 0.3079598441704289313, 0.3333333333333333703, 0.3079598441704289313, 0.3333333333333333703, 0.3079598441704289313, 0.3333333333333333703, 0.3079598441704289313, 0.3333333333333333703, 0.3079598441704289313, 0.3333333333333333703, 0.3079598441704289313, 0.3333333333333333703, 0.3079598441704289313, 0.3333333333333333703, 0.3079598441704289313, 0.3333333333333333703, 0.3079598441704289313, 0.3333333333333333703, 0.3079598441704289313, 0.3333333333333333703, 0.3079598441704289313, 0.3333333333333333703, 0.3079598441704289313, 0.3333333333333333703, 0.3079598441704289313, 0.3333333333333333703, 0.3079598441704289313, 0.3333333333333333703, 0.3079598441704289313, 0.3333333333333333703, 0.3079598441704289313, 0.3333333333333333703, 0.3079598441704289313, 0.3333333333333333703, 0.3079598441704289313, 0.3333333333333333703, 0.3079598441704289313, 0.3333333333333333703, 0.3079598441704289313, 0.3333333333333333703, 0.3079598441704289313, 0.3333333333333333703, 0.3079598441704289313, 0.3333333333333333703, 0.3079598441704289313, 0.3333333333333333703, 0.3079598441704289313, 0.3333333333333333703, 0.3079598441704289313, 0.3333333333333333703, 0.3079598441704289313, 0.3333333333333333703, 0.3079598441704289313, 0.3333333333333333703, 0.3079598441704289313, 0.3333333333333333703, 0.3079598441704289313, 0.3333333333333333703, 0.3079598441704289313, 0.3333333333333333703, 0.3079598441704289313, 0.3333333333333333703, 0.3079598441704289313, 0.3333333333333333703, 0.3079598441704289313, 0.3333333333333333703, 0.3079598441704289313, 0.3333333333333333703),
 ( 1.000000000000000000, 0.9238795325112867385, 1.000000000000000000, 0.9238795325112867385, 1.000000000000000000, 0.9238795325112867385, 1.000000000000000000, 0.9238795325112867385, 1.000000000000000000, 0.9238795325112867385, 1.000000000000000000, 0.9238795325112867385, 1.000000000000000000, 0.9238795325112867385, 1.000000000000000000, 0.9238795325112867385, 1.000000000000000000, 0.9238795325112867385, 1.000000000000000000, 0.9238795325112867385, 1.000000000000000000, 0.9238795325112867385, 1.000000000000000000, 0.9238795325112867385, 1.000000000000000000, 0.9238795325112867385, 1.000000000000000000, 0.9238795325112867385, 1.000000000000000000, 0.9238795325112867385, 1.000000000000000000, 0.9238795325112867385, 1.000000000000000000, 0.9238795325112867385, 1.000000000000000000, 0.9238795325112867385, 1.000000000000000000, 0.9238795325112867385, 1.000000000000000000, 0.9238795325112867385, 1.000000000000000000, 0.9238795325112867385, 1.000000000000000000, 0.9238795325112867385, 1.000000000000000000, 0.9238795325112867385, 1.000000000000000000, 0.9238795325112867385, 1.000000000000000000, 0.9238795325112867385, 1.000000000000000000, 0.9238795325112867385, 1.000000000000000000, 0.9238795325112867385, 1.000000000000000000, 0.9238795325112867385, 1.000000000000000000, 0.9238795325112867385, 1.000000000000000000, 0.9238795325112867385, 1.000000000000000000, 0.9238795325112867385, 1.000000000000000000, 0.9238795325112867385, 1.000000000000000000, 0.9238795325112867385, 1.000000000000000000, 0.9238795325112867385, 1.000000000000000000, 0.9238795325112867385, 1.000000000000000000, 0.9238795325112867385, 1.000000000000000000, 0.9238795325112867385, 1.000000000000000000, 0.9238795325112867385, 1.000000000000000000, 0.9238795325112867385, 1.000000000000000000, 0.9238795325112867385, 1.000000000000000000) ) ) 
 REPRESENTATION_ITEM ( '' )  SURFACE ( )  );
#225 = CARTESIAN_POINT ( 'NONE',  ( -5.249999999999999112, -28.16666666598386826, 3.031088913245538308 ) ) ;
#226 = CARTESIAN_POINT ( 'NONE',  ( 1.045839947578414884E-14, -27.81249999999999289, -5.249999999999999112 ) ) ;
#227 = CARTESIAN_POINT ( 'NONE',  ( -0.01814118441321365544, -0.6493409260993610044, 3.500000000000000000 ) ) ;
#228 = FACE_OUTER_BOUND ( 'NONE', #8574, .T. ) ;
#229 = CARTESIAN_POINT ( 'NONE',  ( 5.385316468749999252, -27.93229166632526628, -3.109213912904139399 ) ) ;
#230 = CARTESIAN_POINT ( 'NONE',  ( -1.674995433905599462, -2.149340926099360782, 3.992485675378533383 ) ) ;
#231 = DIRECTION ( 'NONE',  ( 1.000000000000000000, 0.000000000000000000, -0.000000000000000000 ) ) ;
#232 = ORIENTED_EDGE ( 'NONE', *, *, #8410, .T. ) ;
#233 = CARTESIAN_POINT ( 'NONE',  ( 5.385316468750000141, -27.20312499965860198, -6.595110575850215044E-16 ) ) ;
#234 = CARTESIAN_POINT ( 'NONE',  ( -1.260781871532431708, -5.850659073900641438, -2.992485675378564469 ) ) ;
#235 = ORIENTED_EDGE ( 'NONE', *, *, #430, .T. ) ;
#236 = CARTESIAN_POINT ( 'NONE',  ( 5.250000000000000000, -27.22916666666666430, -3.031088913245534755 ) ) ;
#237 = CARTESIAN_POINT ( 'NONE',  ( -5.114683531250000748, -28.31770833367473728, -2.952963913586935440 ) ) ;
#238 = CARTESIAN_POINT ( 'NONE',  ( -5.249999999999999112, -27.47916666666666430, 3.031088913245538308 ) ) ;
#239 = DIRECTION ( 'NONE',  ( -0.000000000000000000, 1.000000000000000000, -0.000000000000000000 ) ) ;
#240 = CARTESIAN_POINT ( 'NONE',  ( -1.467888652719046449, -3.749340926099360871, 3.492485675378536047 ) ) ;
#241 = DIRECTION ( 'NONE',  ( 0.000000000000000000, -1.000000000000000000, 0.000000000000000000 ) ) ;
#242 = CARTESIAN_POINT ( 'NONE',  ( -5.114683531250000748, -28.27604166700806232, 2.952963913586931888 ) ) ;
#243 = PRESENTATION_STYLE_ASSIGNMENT (( #7268 ) ) ;
#244 = ORIENTED_EDGE ( 'NONE', *, *, #7027, .F. ) ;
#245 = CARTESIAN_POINT ( 'NONE',  ( 6.972266317189433020E-16, -29.43750000000000000, -5.250000000000000000 ) ) ;
#246 = CARTESIAN_POINT ( 'NONE',  ( 2.557341765625000818, -28.31770833367473017, -4.429445870380400052 ) ) ;
#247 = ORIENTED_EDGE ( 'NONE', *, *, #6707, .T. ) ;
#248 = EDGE_CURVE ( 'NONE', #7024, #2834, #3444, .T. ) ;
#249 = CARTESIAN_POINT ( 'NONE',  ( 0.000000000000000000, -27.00000000000000000, -5.250000000000000000 ) ) ;
#250 = CARTESIAN_POINT ( 'NONE',  ( -2.692658234375000514, -28.15104166632526628, -4.663820869356205989 ) ) ;
#251 = CARTESIAN_POINT ( 'NONE',  ( 4.007514324621432422, -3.650659073900639040, 1.638713065079246078 ) ) ;
#252 = CARTESIAN_POINT ( 'NONE',  ( 2.625000000000002220, -29.35416666598386826, 4.546633369868302132 ) ) ;
#253 = CARTESIAN_POINT ( 'NONE',  ( -2.692658234375000514, -27.90104166632526628, -4.663820869356205989 ) ) ;
#254 = ORIENTED_EDGE ( 'NONE', *, *, #8365, .F. ) ;
#255 = CARTESIAN_POINT ( 'NONE',  ( -6.438524027057392246E-16, -29.87813065659485190, 5.257453848358681014 ) ) ;
#256 = CARTESIAN_POINT ( 'NONE',  ( 5.250000000000000000, -29.51041666734946034, -3.031088913245534755 ) ) ;
#257 = PRESENTATION_LAYER_ASSIGNMENT (  '', '', ( #4272 ) ) ;
#258 = CARTESIAN_POINT ( 'NONE',  ( 2.692658234374998738, -27.69270833299193768, -4.663820869356206877 ) ) ;
#259 = CARTESIAN_POINT ( 'NONE',  ( -1.084901341431563923E-15, -27.17187500034140157, 5.905927827173866440 ) ) ;
#260 = ORIENTED_EDGE ( 'NONE', *, *, #6679, .T. ) ;
#261 = CARTESIAN_POINT ( 'NONE',  ( 0.000000000000000000, 1.000000000000000000, -3.999999999999999112 ) ) ;
#262 = CARTESIAN_POINT ( 'NONE',  ( -1.224499502706140497, -4.850659073900639662, 3.007514324621436863 ) ) ;
#263 = DIRECTION ( 'NONE',  ( 0.000000000000000000, 0.000000000000000000, -1.000000000000000000 ) ) ;
#264 = AXIS2_PLACEMENT_3D ( 'NONE', #2417, #8091, #2278 ) ;
#265 = CARTESIAN_POINT ( 'NONE',  ( -5.250000000000000000, -28.43749999931720396, 0.000000000000000000 ) ) ;
#266 = DIRECTION ( 'NONE',  ( 0.000000000000000000, -0.9973637043974449279, -0.07256473765270717025 ) ) ;
#267 = CARTESIAN_POINT ( 'NONE',  ( 0.01814118441321408565, -1.449340926099361271, -3.500000000000000000 ) ) ;
#268 = FACE_OUTER_BOUND ( 'NONE', #8425, .T. ) ;
#269 = DIRECTION ( 'NONE',  ( -1.492469013153037857E-17, 0.9925461516413219831, 0.1218693434051477398 ) ) ;
#270 = CARTESIAN_POINT ( 'NONE',  ( 0.000000000000000000, 0.000000000000000000, 0.000000000000000000 ) ) ;
#271 = CARTESIAN_POINT ( 'NONE',  ( -2.692658234374996518, -28.03645833299193413, 4.663820869356208654 ) ) ;
#272 = CARTESIAN_POINT ( 'NONE',  ( -3.992485675378532939, -6.549340926099361582, -1.674995433905601683 ) ) ;
#273 = CARTESIAN_POINT ( 'NONE',  ( -1.406733260263395735, -29.57366454968462932, 5.250000000000000000 ) ) ;
#274 = ORIENTED_EDGE ( 'NONE', *, *, #6013, .F. ) ;
#275 = CARTESIAN_POINT ( 'NONE',  ( -5.385316468750001029, -28.34895833299193058, -3.109213912904136734 ) ) ;
#276 = CARTESIAN_POINT ( 'NONE',  ( 0.01814118441314514080, -4.950659073900641083, 3.000000000000000444 ) ) ;
#277 = ORIENTED_EDGE ( 'NONE', *, *, #3202, .T. ) ;
#278 = CARTESIAN_POINT ( 'NONE',  ( -5.250000000000000000, -27.87500000000000000, -6.429395695523604153E-16 ) ) ;
#279 = VECTOR ( 'NONE', #5592, 1000.000000000000000 ) ;
#280 = CARTESIAN_POINT ( 'NONE',  ( -1.041183273768722772, -0.07758948893217661180, 3.505490685814065088 ) ) ;
#281 = ORIENTED_EDGE ( 'NONE', *, *, #4233, .T. ) ;
#282 = AXIS2_PLACEMENT_3D ( 'NONE', #7052, #2786, #2167 ) ;
#283 = CARTESIAN_POINT ( 'NONE',  ( -2.557341765625002594, -27.00520833367473017, 4.429445870380399164 ) ) ;
#284 = CARTESIAN_POINT ( 'NONE',  ( 3.616337804771879580E-16, -28.79687500034140157, -5.905927827173866440 ) ) ;
#285 = CARTESIAN_POINT ( 'NONE',  ( -2.487701488670255312, -2.049340926099361582, 2.462045979635577808 ) ) ;
#286 = DIRECTION ( 'NONE',  ( -0.000000000000000000, 1.000000000000000000, -0.000000000000000000 ) ) ;
#287 = CARTESIAN_POINT ( 'NONE',  ( 0.000000000000000000, -30.00000000000000000, 4.250000000000000000 ) ) ;
#288 = CARTESIAN_POINT ( 'NONE',  ( 2.557341765624996821, -29.21354166700806587, 4.429445870380401828 ) ) ;
#289 = CARTESIAN_POINT ( 'NONE',  ( -1.975475456537005874E-15, -27.34375000068279249, 5.250000000000000000 ) ) ;
#290 = EDGE_CURVE ( 'NONE', #6114, #7024, #5977, .T. ) ;
#291 = ORIENTED_EDGE ( 'NONE', *, *, #7027, .T. ) ;
#292 = AXIS2_PLACEMENT_3D ( 'NONE', #3378, #6815, #3894 ) ;
#293 = CARTESIAN_POINT ( 'NONE',  ( -1.406733260263395735, -29.32366454968462932, 5.250000000000000000 ) ) ;
#294 = CARTESIAN_POINT ( 'NONE',  ( 5.114683531249999859, -29.08854166700806942, -2.952963913586932776 ) ) ;
#295 = AXIS2_PLACEMENT_3D ( 'NONE', #3494, #5755, #4370 ) ;
#296 = VERTEX_POINT ( 'NONE', #8506 ) ;
#297 = DIRECTION ( 'NONE',  ( 0.000000000000000000, 0.000000000000000000, 1.000000000000000000 ) ) ;
#298 = DIRECTION ( 'NONE',  ( 0.000000000000000000, 1.000000000000000000, 0.000000000000000000 ) ) ;
#299 = CARTESIAN_POINT ( 'NONE',  ( -4.007514324621431534, -2.850659073900638774, -1.638713065079248521 ) ) ;
#300 = CARTESIAN_POINT ( 'NONE',  ( -5.385316468750001029, -27.88020833299193413, -3.109213912904136734 ) ) ;
#301 = VERTEX_POINT ( 'NONE', #7582 ) ;
#302 = AXIS2_PLACEMENT_3D ( 'NONE', #4792, #7636, #6980 ) ;
#303 = FACE_BOUND ( 'NONE', #8931, .T. ) ;
#304 = CARTESIAN_POINT ( 'NONE',  ( -5.250000000000000000, -29.40625000068279604, -6.429395695523604153E-16 ) ) ;
#305 = CARTESIAN_POINT ( 'NONE',  ( -2.692658234375000514, -28.15104166632526628, -4.663820869356205989 ) ) ;
#306 = PRODUCT_DEFINITION_CONTEXT ( 'detailed design', #4038, 'design' ) ;
#307 = ORIENTED_EDGE ( 'NONE', *, *, #1659, .F. ) ;
#308 = CARTESIAN_POINT ( 'NONE',  ( 0.000000000000000000, -30.00000000000000000, 0.000000000000000000 ) ) ;
#309 = CARTESIAN_POINT ( 'NONE',  ( -2.108492589042352261, -3.150659073900639484, 2.134148098076933397 ) ) ;
#310 = CARTESIAN_POINT ( 'NONE',  ( 1.975475456537005874E-15, -27.43750000000000000, 5.249999999999999112 ) ) ;
#311 = CARTESIAN_POINT ( 'NONE',  ( 5.250000000000000000, -28.54166666598386826, -3.031088913245536531 ) ) ;
#312 = CARTESIAN_POINT ( 'NONE',  ( 0.000000000000000000, -9.000000000000001776, 4.250000000000000000 ) ) ;
#313 = EDGE_CURVE ( 'NONE', #7348, #2202, #1209, .T. ) ;
#314 = CARTESIAN_POINT ( 'NONE',  ( 0.000000000000000000, -27.00000000000000000, 0.000000000000000000 ) ) ;
#315 = CARTESIAN_POINT ( 'NONE',  ( 1.975475456537005874E-15, -28.12499999931720041, 5.249999999999999112 ) ) ;
#316 = DIRECTION ( 'NONE',  ( 1.000000000000000000, 0.000000000000000000, 0.000000000000000000 ) ) ;
#317 = CARTESIAN_POINT ( 'NONE',  ( 5.385316468750000141, -28.20312499965860198, -6.595110575850215044E-16 ) ) ;
#318 = CARTESIAN_POINT ( 'NONE',  ( -4.000000000000000000, -6.649340926099362115, -0.01814118441321865144 ) ) ;
#319 = CARTESIAN_POINT ( 'NONE',  ( -2.624999999999996891, -28.45833333333333215, 4.546633369868304797 ) ) ;
#320 = ORIENTED_EDGE ( 'NONE', *, *, #3522, .T. ) ;
#321 = CARTESIAN_POINT ( 'NONE',  ( 1.142306659890740623E-15, -28.01562499965860553, 6.218427825808274356 ) ) ;
#322 = CARTESIAN_POINT ( 'NONE',  ( 0.01814118441313990887, -6.550659073900639839, 3.500000000000000000 ) ) ;
#323 = ORIENTED_EDGE ( 'NONE', *, *, #5988, .F. ) ;
#324 = CARTESIAN_POINT ( 'NONE',  ( -1.113604000661152470E-15, -28.06249999999999645, 6.062177826491070398 ) ) ;
#325 = CARTESIAN_POINT ( 'NONE',  ( 5.114683531250000748, -26.92187500034139802, 0.000000000000000000 ) ) ;
#326 = ORIENTED_EDGE ( 'NONE', *, *, #7017, .T. ) ;
#327 =( LENGTH_UNIT ( ) NAMED_UNIT ( * ) SI_UNIT ( .MILLI., .METRE. ) );
#328 = CARTESIAN_POINT ( 'NONE',  ( 0.000000000000000000, -47.00000000000000000, 0.000000000000000000 ) ) ;
#329 = EDGE_LOOP ( 'NONE', ( #5209, #4297, #1353, #1594, #6573 ) ) ;
#330 = CARTESIAN_POINT ( 'NONE',  ( -5.114683531250001636, -29.46354166700806232, 2.952963913586931444 ) ) ;
#331 =( BOUNDED_CURVE ( )  B_SPLINE_CURVE ( 2, ( #289, #2486, #200, #3691, #3189, #5309, #5871, #6202, #3416 ),
 .UNSPECIFIED., .F., .F. ) 
 B_SPLINE_CURVE_WITH_KNOTS ( ( 3, 2, 2, 2, 3 ),
 ( 0.8125000000000000000, 0.8194444444444444198, 0.8333333333333333703, 0.8472222222222222099, 0.8541666666666666297 ),
 .UNSPECIFIED. ) 
 CURVE ( )  GEOMETRIC_REPRESENTATION_ITEM ( )  RATIONAL_B_SPLINE_CURVE ( ( 0.9330127018922194093, 0.9330127018922194093, 1.000000000000000000, 0.8660254037844387076, 1.000000000000000000, 0.8660254037844387076, 1.000000000000000000, 0.9330127018922198534, 0.9330127018922192983 ) ) 
 REPRESENTATION_ITEM ( '' )  );
#332 = CARTESIAN_POINT ( 'NONE',  ( -0.01814118441321365544, -5.449340926099361937, 3.500000000000000000 ) ) ;
#333 = CARTESIAN_POINT ( 'NONE',  ( 6.972266317189433020E-16, -28.46875000068279959, -5.250000000000000000 ) ) ;
#334 = CARTESIAN_POINT ( 'NONE',  ( -5.385316468750000141, -30.09374999965860198, 0.000000000000000000 ) ) ;
#335 = CARTESIAN_POINT ( 'NONE',  ( 2.557341765625000818, -28.38020833367473017, -4.429445870380400052 ) ) ;
#336 = AXIS2_PLACEMENT_3D ( 'NONE', #5769, #2196, #6511 ) ;
#337 = FACE_OUTER_BOUND ( 'NONE', #2501, .T. ) ;
#338 = CARTESIAN_POINT ( 'NONE',  ( 5.114683531250000748, -29.90104166700806232, -2.952963913586932776 ) ) ;
#339 = EDGE_LOOP ( 'NONE', ( #7797, #3924, #3008, #7248 ) ) ;
#340 = VECTOR ( 'NONE', #6184, 1000.000000000000000 ) ;
#341 = DIRECTION ( 'NONE',  ( 0.000000000000000000, -0.000000000000000000, 1.000000000000000000 ) ) ;
#342 = CARTESIAN_POINT ( 'NONE',  ( -2.692658234374996518, -29.31770833299193413, 4.663820869356208654 ) ) ;
#343 = CARTESIAN_POINT ( 'NONE',  ( 3.992485675378533383, -0.9493409260993608267, 1.674995433905599462 ) ) ;
#344 = AXIS2_PLACEMENT_3D ( 'NONE', #6374, #8568, #2197 ) ;
#345 = UNCERTAINTY_MEASURE_WITH_UNIT (LENGTH_MEASURE( 1.000000000000000082E-05 ), #5708, 'distance_accuracy_value', 'NONE');
#346 = DIRECTION ( 'NONE',  ( 0.000000000000000000, 1.000000000000000000, 0.000000000000000000 ) ) ;
#347 = CARTESIAN_POINT ( 'NONE',  ( 5.385316468750001029, -28.75520833299193413, 3.109213912904135846 ) ) ;
#348 = EDGE_LOOP ( 'NONE', ( #4332, #2732, #6898, #1040, #4602, #5151, #8448, #421, #7230, #5370, #7405, #1528, #896, #3291, #5973, #7049, #8359, #4121, #7939, #1869, #4062, #7510, #7908, #3823, #5397, #1583, #3967 ) ) ;
#349 = PRODUCT_DEFINITION ( 'UNKNOWN', '', #5751, #3204 ) ;
#350 = DIRECTION ( 'NONE',  ( 0.000000000000000000, 1.000000000000000000, 0.000000000000000000 ) ) ;
#351 = CARTESIAN_POINT ( 'NONE',  ( -2.624999999999998668, -27.94791666734946389, -4.546633369868303021 ) ) ;
#352 = CARTESIAN_POINT ( 'NONE',  ( -5.385316468749998364, -27.58854166632526983, 3.109213912904140287 ) ) ;
#353 = ORIENTED_EDGE ( 'NONE', *, *, #8523, .F. ) ;
#354 = CARTESIAN_POINT ( 'NONE',  ( -2.692658234374996518, -28.03645833299193413, 4.663820869356208654 ) ) ;
#355 = CARTESIAN_POINT ( 'NONE',  ( -3.000000000000000444, -1.350659073900639440, 0.01814118441314532468 ) ) ;
#356 = CARTESIAN_POINT ( 'NONE',  ( 0.000000000000000000, -30.00000000000000000, 0.000000000000000000 ) ) ;
#357 = PRODUCT_DEFINITION_SHAPE ( 'NONE', 'NONE',  #9105 ) ;
#358 = EDGE_CURVE ( 'NONE', #6742, #3365, #4804, .T. ) ;
#359 = CARTESIAN_POINT ( 'NONE',  ( -5.250000000000000000, -28.18749999931720396, 0.000000000000000000 ) ) ;
#360 = CARTESIAN_POINT ( 'NONE',  ( -2.625000000000000444, -28.47916666598386826, -4.546633369868303021 ) ) ;
#361 = CARTESIAN_POINT ( 'NONE',  ( -3.500000000000000000, -0.2493409260993610654, -0.01814118441321343686 ) ) ;
#362 = EDGE_CURVE ( 'NONE', #849, #3341, #1779, .T. ) ;
#363 = CARTESIAN_POINT ( 'NONE',  ( 1.406733260263402174, -27.80133545031536713, 5.249999999999995559 ) ) ;
#364 = PRODUCT_CONTEXT ( 'NONE', #1831, 'mechanical' ) ;
#365 = CARTESIAN_POINT ( 'NONE',  ( 2.692658234374998738, -29.91145833299193413, -4.663820869356206877 ) ) ;
#366 = CARTESIAN_POINT ( 'NONE',  ( -4.000000000000000000, -1.849340926099360738, -0.01814118441321865144 ) ) ;
#367 = EDGE_CURVE ( 'NONE', #5103, #6258, #7983, .T. ) ;
#368 = CARTESIAN_POINT ( 'NONE',  ( -5.385316468750000141, -27.09374999965859843, 0.000000000000000000 ) ) ;
#369 = ORIENTED_EDGE ( 'NONE', *, *, #5900, .T. ) ;
#370 = CARTESIAN_POINT ( 'NONE',  ( 2.692658234375002735, -27.99479166632526628, 4.663820869356205101 ) ) ;
#371 = CARTESIAN_POINT ( 'NONE',  ( 1.431606283892694842, -5.650659073900638596, -3.507514324621434199 ) ) ;
#372 = ORIENTED_EDGE ( 'NONE', *, *, #5983, .F. ) ;
#373 = CARTESIAN_POINT ( 'NONE',  ( 3.712013335537174572E-16, -27.93749999999999645, -6.062177826491070398 ) ) ;
#374 = CARTESIAN_POINT ( 'NONE',  ( 1.406733260263393293, -27.07366454968463287, -5.250000000000000000 ) ) ;
#375 = CARTESIAN_POINT ( 'NONE',  ( -5.114683531250000748, -27.06770833367473017, -2.952963913586935440 ) ) ;
#376 = ORIENTED_EDGE ( 'NONE', *, *, #4348, .F. ) ;
#377 = FACE_OUTER_BOUND ( 'NONE', #6458, .T. ) ;
#378 = EDGE_LOOP ( 'NONE', ( #5714, #6318, #4777, #2554 ) ) ;
#379 = CARTESIAN_POINT ( 'NONE',  ( 5.114683531249998971, -29.63020833367473017, 2.952963913586936329 ) ) ;
#380 = CARTESIAN_POINT ( 'NONE',  ( 0.01814118441321408565, -7.849340926099360516, -3.500000000000000000 ) ) ;
#381 = CARTESIAN_POINT ( 'NONE',  ( -6.972266317189433020E-16, -27.56249999999999645, -5.249999999999999112 ) ) ;
#382 = CARTESIAN_POINT ( 'NONE',  ( -1.406733260263382856, -28.17633545031537068, -5.250000000000006217 ) ) ;
#383 = CARTESIAN_POINT ( 'NONE',  ( 3.616337804771879580E-16, -28.85937500034139802, -5.905927827173866440 ) ) ;
#384 = SURFACE_STYLE_FILL_AREA ( #3326 ) ;
#385 = CARTESIAN_POINT ( 'NONE',  ( -5.250000000000000000, -27.90625000068279604, -6.429395695523604153E-16 ) ) ;
#386 = CARTESIAN_POINT ( 'NONE',  ( -2.557341765624999042, -27.02604166700806232, -4.429445870380400052 ) ) ;
#387 =( BOUNDED_CURVE ( )  B_SPLINE_CURVE ( 2, ( #1018, #3037, #319, #6552, #8833, #8095, #5950, #3912, #3776 ),
 .UNSPECIFIED., .F., .F. ) 
 B_SPLINE_CURVE_WITH_KNOTS ( ( 3, 2, 2, 2, 3 ),
 ( 0.4791666666666666852, 0.4861111111111111049, 0.5000000000000000000, 0.5138888888888888395, 0.5208333333333333703 ),
 .UNSPECIFIED. ) 
 CURVE ( )  GEOMETRIC_REPRESENTATION_ITEM ( )  RATIONAL_B_SPLINE_CURVE ( ( 0.9330127018922194093, 0.9330127018922196314, 1.000000000000000000, 0.8660254037844387076, 1.000000000000000000, 0.8660254037844387076, 1.000000000000000000, 0.9330127018922187432, 0.9330127018922192983 ) ) 
 REPRESENTATION_ITEM ( '' )  );
#388 = EDGE_LOOP ( 'NONE', ( #5734, #5832, #6280, #502 ) ) ;
#389 = FACE_OUTER_BOUND ( 'NONE', #1082, .T. ) ;
#390 = CARTESIAN_POINT ( 'NONE',  ( 2.692658234374998738, -29.44270833299193413, -4.663820869356206877 ) ) ;
#391 = EDGE_CURVE ( 'NONE', #8882, #738, #2591, .T. ) ;
#392 = CARTESIAN_POINT ( 'NONE',  ( -1.406733260263395735, -29.10491455036742536, 5.250000000000000000 ) ) ;
#393 = CARTESIAN_POINT ( 'NONE',  ( 2.625000000000000444, -29.95833333333333215, -4.546633369868303021 ) ) ;
#394 = CARTESIAN_POINT ( 'NONE',  ( 2.692658234375002735, -29.77604166632526983, 4.663820869356205101 ) ) ;
#395 = CARTESIAN_POINT ( 'NONE',  ( -2.841254879263533262, -0.4493409260993607157, 2.815599370228847764 ) ) ;
#396 = EDGE_LOOP ( 'NONE', ( #8293, #5107, #8604, #2518 ) ) ;
#397 = CYLINDRICAL_SURFACE ( 'NONE', #2530, 4.000000000000000000 ) ;
#398 = CARTESIAN_POINT ( 'NONE',  ( -2.625000000000002220, -28.36458333401612819, 4.546633369868302132 ) ) ;
#399 = CARTESIAN_POINT ( 'NONE',  ( -5.385316468750001029, -29.38020833299193413, -3.109213912904136734 ) ) ;
#400 = EDGE_LOOP ( 'NONE', ( #2352, #922 ) ) ;
#401 = CARTESIAN_POINT ( 'NONE',  ( 2.692658234375002735, -28.24479166632526628, 4.663820869356205101 ) ) ;
#402 = CARTESIAN_POINT ( 'NONE',  ( -3.000000000000000444, -6.150659073900639484, 0.01814118441314532468 ) ) ;
#403 = CARTESIAN_POINT ( 'NONE',  ( 2.624999999999996891, -29.54166666666666430, 4.546633369868304797 ) ) ;
#404 = SURFACE_STYLE_FILL_AREA ( #3209 ) ;
#405 = DIRECTION ( 'NONE',  ( -1.000000000000000000, 0.000000000000000000, -0.000000000000000000 ) ) ;
#406 = CARTESIAN_POINT ( 'NONE',  ( 5.114683531250000748, -26.85937500034139802, 0.000000000000000000 ) ) ;
#407 = CARTESIAN_POINT ( 'NONE',  ( 2.557341765624996821, -29.65104166700806232, 4.429445870380401828 ) ) ;
#408 = ORIENTED_EDGE ( 'NONE', *, *, #9125, .F. ) ;
#409 =( GEOMETRIC_REPRESENTATION_CONTEXT ( 3 ) GLOBAL_UNCERTAINTY_ASSIGNED_CONTEXT ( ( #1055 ) ) GLOBAL_UNIT_ASSIGNED_CONTEXT ( ( #5104, #7442, #1066 ) ) REPRESENTATION_CONTEXT ( 'NONE', 'WORKASPACE' ) );
#410 = CARTESIAN_POINT ( 'NONE',  ( -2.692658234375000514, -29.61979166632526983, -4.663820869356205989 ) ) ;
#411 = CARTESIAN_POINT ( 'NONE',  ( 2.462045979635577364, -4.049340926099360694, 2.487701488670255312 ) ) ;
#412 = CARTESIAN_POINT ( 'NONE',  ( 5.250000000000000000, -26.89062500034139802, 0.000000000000000000 ) ) ;
#413 = CARTESIAN_POINT ( 'NONE',  ( 2.692658234374998738, -28.41145833299193413, -4.663820869356206877 ) ) ;
#414 = CARTESIAN_POINT ( 'NONE',  ( 3.492485675378566690, -7.050659073900641616, -1.467888652718972287 ) ) ;
#415 = ORIENTED_EDGE ( 'NONE', *, *, #2354, .T. ) ;
#416 = CARTESIAN_POINT ( 'NONE',  ( 2.300847884672513123E-14, -27.21875000068279959, -5.250000000000000000 ) ) ;
#417 = ADVANCED_BREP_SHAPE_REPRESENTATION ( '', ( #8468, #888 ), #7729 ) ;
#418 = LINE ( 'NONE', #4145, #7439 ) ;
#419 = ADVANCED_FACE ( 'NONE', ( #7237, #2173 ), #774, .T. ) ;
#420 = CARTESIAN_POINT ( 'NONE',  ( 3.492485675378566690, -0.6506590739006392621, -1.467888652718972287 ) ) ;
#421 = ORIENTED_EDGE ( 'NONE', *, *, #2572, .T. ) ;
#422 = CARTESIAN_POINT ( 'NONE',  ( 5.250000000000000000, -28.35416666666666785, -3.031088913245536531 ) ) ;
#423 = ORIENTED_EDGE ( 'NONE', *, *, #8631, .F. ) ;
#424 = AXIS2_PLACEMENT_3D ( 'NONE', #4231, #5705, #777 ) ;
#425 = CARTESIAN_POINT ( 'NONE',  ( 5.114683531250000748, -28.85937500034139802, 0.000000000000000000 ) ) ;
#426 = CARTESIAN_POINT ( 'NONE',  ( -1.260781871532494103, -0.5493409260993613596, 2.992485675378538712 ) ) ;
#427 = LINE ( 'NONE', #7410, #8373 ) ;
#428 = CARTESIAN_POINT ( 'NONE',  ( -5.114683531250000748, -29.02604166700806587, 2.952963913586931888 ) ) ;
#429 = CARTESIAN_POINT ( 'NONE',  ( -5.249999999999999112, -29.20833333265053611, -3.031088913245534755 ) ) ;
#430 = EDGE_CURVE ( 'NONE', #3312, #7207, #3019, .T. ) ;
#431 = CARTESIAN_POINT ( 'NONE',  ( -2.624999999999998668, -27.94791666734946389, -4.546633369868303021 ) ) ;
#432 = CARTESIAN_POINT ( 'NONE',  ( 0.000000000000000000, -30.00000000000000000, 0.000000000000000000 ) ) ;
#433 = AXIS2_PLACEMENT_3D ( 'NONE', #4506, #7382, #7240 ) ;
#434 = CARTESIAN_POINT ( 'NONE',  ( -1.406733260263395735, -28.32366454968462577, 5.250000000000000000 ) ) ;
#435 = EDGE_CURVE ( 'NONE', #6343, #8584, #1529, .T. ) ;
#436 = CARTESIAN_POINT ( 'NONE',  ( 5.114683531250000748, -29.67187500034139802, 0.000000000000000000 ) ) ;
#437 = ORIENTED_EDGE ( 'NONE', *, *, #2736, .F. ) ;
#438 = DIRECTION ( 'NONE',  ( -0.000000000000000000, -1.000000000000000000, -0.000000000000000000 ) ) ;
#439 = CARTESIAN_POINT ( 'NONE',  ( 5.385316468750000141, -28.23437499965860198, -6.595110575850215044E-16 ) ) ;
#440 = CARTESIAN_POINT ( 'NONE',  ( 9.180150650966086169E-15, -28.56249999999999645, 5.250000000000000000 ) ) ;
#441 = LINE ( 'NONE', #9040, #870 ) ;
#442 = CARTESIAN_POINT ( 'NONE',  ( 2.692658234374998738, -29.44270833299193413, -4.663820869356206877 ) ) ;
#443 = CIRCLE ( 'NONE', #7579, 2.500000000000000000 ) ;
#444 = CARTESIAN_POINT ( 'NONE',  ( -1.638713065079163034, -6.349340926099361404, -4.007514324621466173 ) ) ;
#445 = ORIENTED_EDGE ( 'NONE', *, *, #3049, .T. ) ;
#446=STYLED_ITEM('',(#9211),#2174);
#447 = DIRECTION ( 'NONE',  ( -0.000000000000000000, -1.000000000000000000, -0.000000000000000000 ) ) ;
#448 = CARTESIAN_POINT ( 'NONE',  ( -5.250000000000000000, -27.92708333401612819, -3.031088913245536531 ) ) ;
#449 = CARTESIAN_POINT ( 'NONE',  ( -5.385316468750000141, -29.60937499965859843, 0.000000000000000000 ) ) ;
#450 = VECTOR ( 'NONE', #5852, 1000.000000000000000 ) ;
#451 = VERTEX_POINT ( 'NONE', #8588 ) ;
#452 = CARTESIAN_POINT ( 'NONE',  ( -5.385316468750001029, -28.09895833299192702, -3.109213912904136734 ) ) ;
#453 = CARTESIAN_POINT ( 'NONE',  ( -0.01814118441313947866, -2.550659073900638951, -3.500000000000000000 ) ) ;
#454 = CARTESIAN_POINT ( 'NONE',  ( 0.000000000000000000, 69.99999999999998579, 0.000000000000000000 ) ) ;
#455 = VECTOR ( 'NONE', #7883, 1000.000000000000000 ) ;
#456 =( NAMED_UNIT ( * ) SI_UNIT ( $, .STERADIAN. ) SOLID_ANGLE_UNIT ( ) );
#457 = CARTESIAN_POINT ( 'NONE',  ( 1.975475456537005874E-15, -27.18750000000000000, 5.249999999999999112 ) ) ;
#458 = CARTESIAN_POINT ( 'NONE',  ( 1.975475456537005874E-15, -27.43750000000000000, 5.250000000000000000 ) ) ;
#459 = CARTESIAN_POINT ( 'NONE',  ( 2.557341765625000818, -29.31770833367473017, -4.429445870380400052 ) ) ;
#460 = ORIENTED_EDGE ( 'NONE', *, *, #7717, .T. ) ;
#461 = APPLICATION_PROTOCOL_DEFINITION ( 'draft international standard', 'automotive_design', 1998, #43 ) ;
#462 = CARTESIAN_POINT ( 'NONE',  ( -2.692658234375000514, -29.86979166632526983, -4.663820869356205989 ) ) ;
#463 = CARTESIAN_POINT ( 'NONE',  ( 2.487701488670255756, -7.649340926099361226, -2.462045979635577364 ) ) ;
#464 = DIRECTION ( 'NONE',  ( -0.000000000000000000, -1.000000000000000000, -0.000000000000000000 ) ) ;
#465 = CARTESIAN_POINT ( 'NONE',  ( 5.385316468750001029, -28.97395833299193413, 3.109213912904135846 ) ) ;
#466 = CARTESIAN_POINT ( 'NONE',  ( 2.462045979635629767, -3.950659073900639751, -2.487701488670203354 ) ) ;
#467 = VECTOR ( 'NONE', #3569, 1000.000000000000000 ) ;
#468 = ORIENTED_EDGE ( 'NONE', *, *, #7764, .T. ) ;
#469 = CARTESIAN_POINT ( 'NONE',  ( 2.143131898507868051E-16, -53.00000000000000000, -1.749999999999999778 ) ) ;
#470 = CARTESIAN_POINT ( 'NONE',  ( 2.487701488670203354, -3.550659073900638951, 2.462045979635629323 ) ) ;
#471 =( BOUNDED_CURVE ( )  B_SPLINE_CURVE ( 2, ( #670, #9175, #628, #9136, #1283, #3603, #5600, #2161, #6260 ),
 .UNSPECIFIED., .F., .T. ) 
 B_SPLINE_CURVE_WITH_KNOTS ( ( 3, 2, 2, 2, 3 ),
 ( 0.6875000000000000000, 0.6944444444444444198, 0.7083333333333333703, 0.7222222222222222099, 0.7291666666666667407 ),
 .UNSPECIFIED. ) 
 CURVE ( )  GEOMETRIC_REPRESENTATION_ITEM ( )  RATIONAL_B_SPLINE_CURVE ( ( 0.9330127018922194093, 0.9330127018922194093, 1.000000000000000000, 0.8660254037844387076, 1.000000000000000000, 0.8660254037844387076, 1.000000000000000000, 0.9330127018922187432, 0.9330127018922192983 ) ) 
 REPRESENTATION_ITEM ( '' )  );
#472 = ORIENTED_EDGE ( 'NONE', *, *, #8246, .T. ) ;
#473 =( LENGTH_UNIT ( ) NAMED_UNIT ( * ) SI_UNIT ( .MILLI., .METRE. ) );
#474 = CARTESIAN_POINT ( 'NONE',  ( 2.625000000000002220, -28.16666666666666785, 4.546633369868302132 ) ) ;
#475 = ORIENTED_EDGE ( 'NONE', *, *, #2084, .T. ) ;
#476 = CARTESIAN_POINT ( 'NONE',  ( -5.114683531250001636, -29.21354166700806587, 2.952963913586931444 ) ) ;
#477 = CARTESIAN_POINT ( 'NONE',  ( -0.01814118441321365544, -7.049340926099361582, 3.500000000000000000 ) ) ;
#478 = FACE_OUTER_BOUND ( 'NONE', #6239, .T. ) ;
#479 = CARTESIAN_POINT ( 'NONE',  ( -5.114683531250000748, -27.79687500034139802, -6.263680815196995234E-16 ) ) ;
#480 = CARTESIAN_POINT ( 'NONE',  ( -2.624999999999996891, -29.14583333265053611, 4.546633369868304797 ) ) ;
#481 = ADVANCED_FACE ( 'NONE', ( #820 ), #7102, .F. ) ;
#482 = CARTESIAN_POINT ( 'NONE',  ( 2.300847884672513123E-14, -27.96875000068279959, -5.250000000000000000 ) ) ;
#483 = DIRECTION ( 'NONE',  ( 0.000000000000000000, 1.000000000000000000, 0.000000000000000000 ) ) ;
#484 = CARTESIAN_POINT ( 'NONE',  ( 0.000000000000000000, -30.00000000000000000, 0.000000000000000000 ) ) ;
#485 = CARTESIAN_POINT ( 'NONE',  ( -2.557341765624999042, -29.58854166700806232, -4.429445870380400052 ) ) ;
#486 = ADVANCED_FACE ( 'NONE', ( #726 ), #5094, .F. ) ;
#487 = PLANE ( 'NONE',  #4222 ) ;
#488 = CARTESIAN_POINT ( 'NONE',  ( -2.692658234374996518, -28.56770833299193413, 4.663820869356208654 ) ) ;
#489 = CARTESIAN_POINT ( 'NONE',  ( -5.385316468750000141, -29.60937499965859843, 0.000000000000000000 ) ) ;
#490 = CARTESIAN_POINT ( 'NONE',  ( 0.000000000000000000, -9.999999999999998224, 0.000000000000000000 ) ) ;
#491 = CARTESIAN_POINT ( 'NONE',  ( 2.692658234375002735, -28.77604166632526628, 4.663820869356205101 ) ) ;
#492 = CARTESIAN_POINT ( 'NONE',  ( 1.467888652719048226, -2.949340926099361493, -3.492485675378536047 ) ) ;
#493 = CARTESIAN_POINT ( 'NONE',  ( -2.815599370228846876, -6.449340926099361049, -2.841254879263533262 ) ) ;
#494 = VECTOR ( 'NONE', #3689, 1000.000000000000000 ) ;
#495 = ORIENTED_EDGE ( 'NONE', *, *, #3861, .T. ) ;
#496 = ADVANCED_FACE ( 'NONE', ( #7809 ), #224, .T. ) ;
#497 = CARTESIAN_POINT ( 'NONE',  ( 2.625000000000000444, -29.23958333401613174, -4.546633369868303021 ) ) ;
#498 = CARTESIAN_POINT ( 'NONE',  ( 5.250000000000000000, -27.78125000068279604, 0.000000000000000000 ) ) ;
#499 = CARTESIAN_POINT ( 'NONE',  ( 5.385316468750001029, -29.75520833299193413, 3.109213912904135846 ) ) ;
#500 = AXIS2_PLACEMENT_3D ( 'NONE', #4103, #6277, #6092 ) ;
#501 =( GEOMETRIC_REPRESENTATION_CONTEXT ( 3 ) GLOBAL_UNCERTAINTY_ASSIGNED_CONTEXT ( ( #1749 ) ) GLOBAL_UNIT_ASSIGNED_CONTEXT ( ( #4938, #8573, #8161 ) ) REPRESENTATION_CONTEXT ( 'NONE', 'WORKASPACE' ) );
#502 = ORIENTED_EDGE ( 'NONE', *, *, #1398, .F. ) ;
#503 = CARTESIAN_POINT ( 'NONE',  ( -2.692658234374996518, -28.53645833299193413, 4.663820869356208654 ) ) ;
#504 = CARTESIAN_POINT ( 'NONE',  ( 1.467888652718972731, -3.450659073900638862, 3.492485675378566246 ) ) ;
#505 = CARTESIAN_POINT ( 'NONE',  ( 2.625000000000000444, -29.73958333401613174, -4.546633369868303021 ) ) ;
#506 = AXIS2_PLACEMENT_3D ( 'NONE', #1402, #9122, #6460 ) ;
#507 = CARTESIAN_POINT ( 'NONE',  ( 4.898587196589412829E-16, 73.00000000000001421, 4.000000000000000000 ) ) ;
#508 = DIRECTION ( 'NONE',  ( 0.000000000000000000, 1.000000000000000000, 0.000000000000000000 ) ) ;
#509 = CARTESIAN_POINT ( 'NONE',  ( -3.507514324621464397, -6.749340926099361759, 1.431606283892619569 ) ) ;
#510 = FACE_OUTER_BOUND ( 'NONE', #109, .T. ) ;
#511 = DIRECTION ( 'NONE',  ( 0.000000000000000000, 0.000000000000000000, -1.000000000000000000 ) ) ;
#512 = CARTESIAN_POINT ( 'NONE',  ( -2.692658234375000514, -29.36979166632526983, -4.663820869356205989 ) ) ;
#513 = EDGE_CURVE ( 'NONE', #1200, #7933, #6888, .T. ) ;
#514 = CARTESIAN_POINT ( 'NONE',  ( -1.431606283892620235, -6.349340926099360516, -3.507514324621463953 ) ) ;
#515 = FACE_OUTER_BOUND ( 'NONE', #8742, .T. ) ;
#516 = CARTESIAN_POINT ( 'NONE',  ( -2.692658234374996518, -29.53645833299193413, 4.663820869356208654 ) ) ;
#517 = EDGE_CURVE ( 'NONE', #2565, #5103, #5524, .T. ) ;
#518 = CARTESIAN_POINT ( 'NONE',  ( 2.487701488670203354, -3.550659073900638951, 2.462045979635629323 ) ) ;
#519 = EDGE_LOOP ( 'NONE', ( #1240, #6626, #8877, #4519 ) ) ;
#520 = FACE_OUTER_BOUND ( 'NONE', #7413, .T. ) ;
#521 = DIRECTION ( 'NONE',  ( 0.000000000000000000, 0.000000000000000000, -1.000000000000000000 ) ) ;
#522 = CARTESIAN_POINT ( 'NONE',  ( 3.500000000000000000, -5.350659073900638774, -0.01814118441313969030 ) ) ;
#523 = ORIENTED_EDGE ( 'NONE', *, *, #4456, .T. ) ;
#524 = CARTESIAN_POINT ( 'NONE',  ( 5.250000000000000888, -28.39583333333333215, 3.031088913245532979 ) ) ;
#525 = APPLICATION_CONTEXT ( 'automotive_design' ) ;
#526 = CARTESIAN_POINT ( 'NONE',  ( -1.084901341431563726E-15, -27.42187500034139802, 5.905927827173866440 ) ) ;
#527 = CARTESIAN_POINT ( 'NONE',  ( 2.462045979635577364, -7.249340926099360871, 2.487701488670255312 ) ) ;
#528 = DIRECTION ( 'NONE',  ( 0.000000000000000000, 0.000000000000000000, 1.000000000000000000 ) ) ;
#529 = CARTESIAN_POINT ( 'NONE',  ( 5.114683531249998971, -27.44270833367473017, 2.952963913586936329 ) ) ;
#530 = CARTESIAN_POINT ( 'NONE',  ( -5.250000000000000000, -30.00000000000000000, 0.000000000000000000 ) ) ;
#531 =( BOUNDED_CURVE ( )  B_SPLINE_CURVE ( 2, ( #361, #7438, #3211, #2413, #227, #6638, #177, #5198, #7991, #1813, #7388, #1621, #267, #6730, #5244, #8784, #8088, #2368, #5288, #7341, #5942, #966, #4644, #871, #4458, #3860, #6682, #4600, #1715, #3075, #4512, #8690, #3029, #7296, #6029, #920, #4554, #3166, #3770, #3720, #8040, #5896, #6545, #3120, #1765, #8828, #8736, #3813, #5987, #2463, #8137, #8868, #6597, #1063, #3907, #5851, #2507, #1669, #5569, #2748, #554, #3953, #4092, #4782, #1293, #509, #3397, #1999, #2700, #8276, #6078, #3352, #4134, #1113, #6182, #6131, #5528, #6225, #8414, #6928, #7624 ),
 .UNSPECIFIED., .F., .T. ) 
 B_SPLINE_CURVE_WITH_KNOTS ( ( 3, 2, 2, 2, 2, 2, 2, 2, 2, 2, 2, 2, 2, 2, 2, 2, 2, 2, 2, 2, 2, 2, 2, 2, 2, 2, 2, 2, 2, 2, 2, 2, 2, 2, 2, 2, 2, 2, 2, 2, 3 ),
 ( 0.000000000000000000, 0.02500000000000000139, 0.05000000000000000278, 0.07499999999999999722, 0.1000000000000000056, 0.1250000000000000000, 0.1499999999999999944, 0.1749999999999999889, 0.2000000000000000111, 0.2250000000000000056, 0.2500000000000000000, 0.2750000000000000222, 0.2999999999999999889, 0.3250000000000000111, 0.3499999999999999778, 0.3750000000000000000, 0.4000000000000000222, 0.4249999999999999889, 0.4500000000000000111, 0.4749999999999999778, 0.5000000000000000000, 0.5250000000000000222, 0.5500000000000000444, 0.5749999999999999556, 0.5999999999999999778, 0.6250000000000000000, 0.6500000000000000222, 0.6750000000000000444, 0.6999999999999999556, 0.7249999999999999778, 0.7500000000000000000, 0.7750000000000000222, 0.8000000000000000444, 0.8249999999999999556, 0.8499999999999999778, 0.8750000000000000000, 0.9000000000000000222, 0.9250000000000000444, 0.9499999999999999556, 0.9749999999999999778, 1.000000000000000000 ),
 .UNSPECIFIED. ) 
 CURVE ( )  GEOMETRIC_REPRESENTATION_ITEM ( )  RATIONAL_B_SPLINE_CURVE ( ( 1.000000000000000000, 0.9238795325112867385, 1.000000000000000000, 0.9238795325112867385, 1.000000000000000000, 0.9238795325112867385, 1.000000000000000000, 0.9238795325112867385, 1.000000000000000000, 0.9238795325112867385, 1.000000000000000000, 0.9238795325112867385, 1.000000000000000000, 0.9238795325112867385, 1.000000000000000000, 0.9238795325112867385, 1.000000000000000000, 0.9238795325112867385, 1.000000000000000000, 0.9238795325112867385, 1.000000000000000000, 0.9238795325112867385, 1.000000000000000000, 0.9238795325112867385, 1.000000000000000000, 0.9238795325112867385, 1.000000000000000000, 0.9238795325112867385, 1.000000000000000000, 0.9238795325112867385, 1.000000000000000000, 0.9238795325112867385, 1.000000000000000000, 0.9238795325112867385, 1.000000000000000000, 0.9238795325112867385, 1.000000000000000000, 0.9238795325112867385, 1.000000000000000000, 0.9238795325112867385, 1.000000000000000000, 0.9238795325112867385, 1.000000000000000000, 0.9238795325112867385, 1.000000000000000000, 0.9238795325112867385, 1.000000000000000000, 0.9238795325112867385, 1.000000000000000000, 0.9238795325112867385, 1.000000000000000000, 0.9238795325112867385, 1.000000000000000000, 0.9238795325112867385, 1.000000000000000000, 0.9238795325112867385, 1.000000000000000000, 0.9238795325112867385, 1.000000000000000000, 0.9238795325112867385, 1.000000000000000000, 0.9238795325112867385, 1.000000000000000000, 0.9238795325112867385, 1.000000000000000000, 0.9238795325112867385, 1.000000000000000000, 0.9238795325112867385, 1.000000000000000000, 0.9238795325112867385, 1.000000000000000000, 0.9238795325112867385, 1.000000000000000000, 0.9238795325112867385, 1.000000000000000000, 0.9238795325112867385, 1.000000000000000000, 0.9238795325112867385, 1.000000000000000000, 0.9238795325112867385, 1.000000000000000000 ) ) 
 REPRESENTATION_ITEM ( '' )  );
#532 = CARTESIAN_POINT ( 'NONE',  ( 3.616337804771879580E-16, -29.60937500034139447, -5.905927827173866440 ) ) ;
#533 = CARTESIAN_POINT ( 'NONE',  ( 0.000000000000000000, 70.00000000000000000, 0.000000000000000000 ) ) ;
#534 = CARTESIAN_POINT ( 'NONE',  ( -5.114683531250000748, -28.54687500034139802, -6.263680815196995234E-16 ) ) ;
#535 = CARTESIAN_POINT ( 'NONE',  ( -5.385316468749998364, -29.08854166632526983, 3.109213912904140287 ) ) ;
#536 = CARTESIAN_POINT ( 'NONE',  ( 2.692658234374998738, -29.69270833299193413, -4.663820869356206877 ) ) ;
#537 = DIRECTION ( 'NONE',  ( 0.000000000000000000, 0.000000000000000000, 1.000000000000000000 ) ) ;
#538 = CARTESIAN_POINT ( 'NONE',  ( 5.385316468750000141, -28.98437499965859843, -6.595110575850215044E-16 ) ) ;
#539 = CARTESIAN_POINT ( 'NONE',  ( 2.487701488670255756, -6.049340926099361582, -2.462045979635577364 ) ) ;
#540 = CARTESIAN_POINT ( 'NONE',  ( 3.992485675378533383, -5.749340926099361759, 1.674995433905599462 ) ) ;
#541 = ORIENTED_EDGE ( 'NONE', *, *, #4558, .F. ) ;
#542 = ADVANCED_BREP_SHAPE_REPRESENTATION ( '', ( #8451, #888 ), #3388 ) ;
#543 = CARTESIAN_POINT ( 'NONE',  ( 0.000000000000000000, 69.99999999999998579, 0.000000000000000000 ) ) ;
#544 = CARTESIAN_POINT ( 'NONE',  ( -1.113604000661152470E-15, -28.34375000068279249, 6.062177826491070398 ) ) ;
#545 = CARTESIAN_POINT ( 'NONE',  ( -2.692658234375000514, -28.65104166632526628, -4.663820869356205989 ) ) ;
#546 = EDGE_CURVE ( 'NONE', #27, #4503, #1592, .T. ) ;
#547 = ORIENTED_EDGE ( 'NONE', *, *, #6137, .F. ) ;
#548 = CARTESIAN_POINT ( 'NONE',  ( 5.385316468750000141, -28.20312499965860198, -6.595110575850215044E-16 ) ) ;
#549 = CARTESIAN_POINT ( 'NONE',  ( -1.431606283892693066, -1.650659073900638818, 3.507514324621434199 ) ) ;
#550 = CARTESIAN_POINT ( 'NONE',  ( 5.250000000000000000, -29.50000000000000000, 0.000000000000000000 ) ) ;
#551 = DIRECTION ( 'NONE',  ( 0.000000000000000000, -1.000000000000000000, 0.000000000000000000 ) ) ;
#552 = LINE ( 'NONE', #1253, #8953 ) ;
#553 = ADVANCED_FACE ( 'NONE', ( #4389 ), #8133, .T. ) ;
#554 = CARTESIAN_POINT ( 'NONE',  ( 0.01814118441321408565, -6.249340926099360871, -3.500000000000000000 ) ) ;
#555 = CARTESIAN_POINT ( 'NONE',  ( -1.084901341431563923E-15, -29.67187500034139802, 5.905927827173866440 ) ) ;
#556 = CARTESIAN_POINT ( 'NONE',  ( 1.406733260263402174, -27.58258545099816317, 5.249999999999995559 ) ) ;
#557 = APPLICATION_PROTOCOL_DEFINITION ( 'draft international standard', 'automotive_design', 1998, #8005 ) ;
#558 = CARTESIAN_POINT ( 'NONE',  ( -5.385316468750001029, -29.34895833299193413, -3.109213912904136734 ) ) ;
#559 = CARTESIAN_POINT ( 'NONE',  ( 1.467888652719048226, -4.549340926099360694, -3.492485675378536047 ) ) ;
#560 = CYLINDRICAL_SURFACE ( 'NONE', #5921, 5.250000000000000000 ) ;
#561 = CARTESIAN_POINT ( 'NONE',  ( -2.692658234374996518, -27.31770833299193413, 4.663820869356208654 ) ) ;
#562 = CARTESIAN_POINT ( 'NONE',  ( 2.815599370228907716, -2.350659073900638774, -2.841254879263473310 ) ) ;
#563 = DIRECTION ( 'NONE',  ( 0.000000000000000000, 0.000000000000000000, -1.000000000000000000 ) ) ;
#564 = CYLINDRICAL_SURFACE ( 'NONE', #5351, 5.250000000000000000 ) ;
#565 = PRODUCT_DEFINITION_FORMATION_WITH_SPECIFIED_SOURCE ( 'ANY', '', #2108, .NOT_KNOWN. ) ;
#566 = VERTEX_POINT ( 'NONE', #5578 ) ;
#567 = CARTESIAN_POINT ( 'NONE',  ( 2.624999999999998668, -28.33333333333333215, -4.546633369868303021 ) ) ;
#568 = CARTESIAN_POINT ( 'NONE',  ( -1.084901341431563726E-15, -28.17187500034139447, 5.905927827173866440 ) ) ;
#569 = CARTESIAN_POINT ( 'NONE',  ( -0.01814118441320841310, -0.6493409260993614485, 3.000000000000000444 ) ) ;
#570 = CARTESIAN_POINT ( 'NONE',  ( 5.250000000000000000, -28.12500000000000000, -6.429395695523604153E-16 ) ) ;
#571 = CARTESIAN_POINT ( 'NONE',  ( -5.250000000000000000, -29.89583333333333215, -3.031088913245536531 ) ) ;
#572 = FACE_OUTER_BOUND ( 'NONE', #9117, .T. ) ;
#573 = CARTESIAN_POINT ( 'NONE',  ( -5.114683531250001636, -28.77604166700806587, 2.952963913586931444 ) ) ;
#574 = VECTOR ( 'NONE', #6967, 1000.000000000000000 ) ;
#575 = AXIS2_PLACEMENT_3D ( 'NONE', #8304, #7511, #3982 ) ;
#576 = CARTESIAN_POINT ( 'NONE',  ( -5.114683531250000748, -29.52604166700806232, 2.952963913586931888 ) ) ;
#577 = CARTESIAN_POINT ( 'NONE',  ( -5.249999999999997335, -29.22916666666666785, 3.031088913245538308 ) ) ;
#578 = ADVANCED_FACE ( 'NONE', ( #8381, #5440 ), #8422, .T. ) ;
#579 = CARTESIAN_POINT ( 'NONE',  ( -3.712013335537174572E-16, -28.74999999931720396, -6.062177826491070398 ) ) ;
#580 = CARTESIAN_POINT ( 'NONE',  ( -2.692658234375000514, -29.65104166632526983, -4.663820869356205989 ) ) ;
#581 = FILL_AREA_STYLE ('',( #8399 ) ) ;
#582 = CARTESIAN_POINT ( 'NONE',  ( 0.000000000000000000, 74.00000000000001421, 2.500000000000000000 ) ) ;
#583 = CARTESIAN_POINT ( 'NONE',  ( 2.487701488670255756, -2.849340926099361404, -2.462045979635577364 ) ) ;
#584 = CARTESIAN_POINT ( 'NONE',  ( 3.500000000000000000, -2.649340926099361226, 0.01814118441321387054 ) ) ;
#585 = EDGE_LOOP ( 'NONE', ( #8972, #8285, #6547 ) ) ;
#586 = AXIS2_PLACEMENT_3D ( 'NONE', #3012, #4443, #8023 ) ;
#587 = FACE_BOUND ( 'NONE', #2803, .T. ) ;
#588 = CARTESIAN_POINT ( 'NONE',  ( -1.113604000661152470E-15, -27.34375000068279959, 6.062177826491070398 ) ) ;
#589 = CARTESIAN_POINT ( 'NONE',  ( 2.692658234374998738, -28.94270833299193413, -4.663820869356206877 ) ) ;
#590 = ORIENTED_EDGE ( 'NONE', *, *, #1735, .F. ) ;
#591 = AXIS2_PLACEMENT_3D ( 'NONE', #8216, #7514, #537 ) ;
#592 = CARTESIAN_POINT ( 'NONE',  ( 1.142306659890740623E-15, -29.01562499965860198, 6.218427825808274356 ) ) ;
#593 = CARTESIAN_POINT ( 'NONE',  ( -1.224499502706140497, -6.450659073900641971, 3.007514324621436863 ) ) ;
#594 = FACE_OUTER_BOUND ( 'NONE', #5132, .T. ) ;
#595 = CARTESIAN_POINT ( 'NONE',  ( -5.317658234375000070, -27.03906249982929921, 0.000000000000000000 ) ) ;
#596 = CARTESIAN_POINT ( 'NONE',  ( 0.000000000000000000, -53.00000000000000000, 0.000000000000000000 ) ) ;
#597 = FACE_OUTER_BOUND ( 'NONE', #7205, .T. ) ;
#598 = CARTESIAN_POINT ( 'NONE',  ( 3.616337804771879580E-16, -29.04687500034139802, -5.905927827173866440 ) ) ;
#599 = DIRECTION ( 'NONE',  ( -0.000000000000000000, 1.000000000000000000, -0.000000000000000000 ) ) ;
#600 = AXIS2_PLACEMENT_3D ( 'NONE', #1254, #6968, #5476 ) ;
#601 = CARTESIAN_POINT ( 'NONE',  ( -2.625000000000000444, -28.72916666598386826, -4.546633369868303021 ) ) ;
#602 = CARTESIAN_POINT ( 'NONE',  ( -3.007514324621463508, -0.3493409260993614596, 1.224499502706077658 ) ) ;
#603 = LINE ( 'NONE', #412, #1926 ) ;
#604 = CARTESIAN_POINT ( 'NONE',  ( -3.807688866302469071E-16, -29.39062499965860198, -6.218427825808274356 ) ) ;
#605 = CARTESIAN_POINT ( 'NONE',  ( -2.815599370228907272, -4.750659073900638241, 2.841254879263473754 ) ) ;
#606 = DIRECTION ( 'NONE',  ( 0.000000000000000000, -1.000000000000000000, 0.000000000000000000 ) ) ;
#607 = CIRCLE ( 'NONE', #1956, 2.786798956483056422 ) ;
#608 = CYLINDRICAL_SURFACE ( 'NONE', #8342, 5.250000000000000000 ) ;
#609 = EDGE_CURVE ( 'NONE', #3341, #6499, #9020, .T. ) ;
#610 = VERTEX_POINT ( 'NONE', #1167 ) ;
#611 = CARTESIAN_POINT ( 'NONE',  ( -3.712013335537174572E-16, -27.81250000000000000, -6.062177826491070398 ) ) ;
#612 = CIRCLE ( 'NONE', #2974, 3.000000000000000444 ) ;
#613 = CARTESIAN_POINT ( 'NONE',  ( -1.084901341431563726E-15, -27.17187500034139802, 5.905927827173866440 ) ) ;
#614 = CARTESIAN_POINT ( 'NONE',  ( -1.224499502706077880, -6.349340926099361404, -3.007514324621463064 ) ) ;
#615 = CARTESIAN_POINT ( 'NONE',  ( 2.557341765625000818, -27.38020833367473017, -4.429445870380400052 ) ) ;
#616 = DIRECTION ( 'NONE',  ( 0.000000000000000000, 1.000000000000000000, 0.000000000000000000 ) ) ;
#617 = CARTESIAN_POINT ( 'NONE',  ( -5.114683531250000748, -29.56770833367472662, -2.952963913586935440 ) ) ;
#618 = SURFACE_SIDE_STYLE ('',( #6992 ) ) ;
#619 = CARTESIAN_POINT ( 'NONE',  ( -1.084901341431563923E-15, -28.73437500034139802, 5.905927827173866440 ) ) ;
#620 = CARTESIAN_POINT ( 'NONE',  ( -2.624999999999998668, -29.66666666666666430, -4.546633369868303021 ) ) ;
#621 = CARTESIAN_POINT ( 'NONE',  ( 5.250000000000000000, -28.79166666598386826, -3.031088913245536531 ) ) ;
#622 = CARTESIAN_POINT ( 'NONE',  ( -2.487701488670255312, -0.4493409260993610488, 2.462045979635577808 ) ) ;
#623 =( NAMED_UNIT ( * ) SI_UNIT ( $, .STERADIAN. ) SOLID_ANGLE_UNIT ( ) );
#624 = DIRECTION ( 'NONE',  ( 0.000000000000000000, 0.000000000000000000, -1.000000000000000000 ) ) ;
#625 = CARTESIAN_POINT ( 'NONE',  ( -4.000000000000000000, -8.249340926099360871, -0.01814118441321865144 ) ) ;
#626 = CARTESIAN_POINT ( 'NONE',  ( 3.500000000000000000, -1.049340926099360916, 0.01814118441321387054 ) ) ;
#627 = VERTEX_POINT ( 'NONE', #4875 ) ;
#628 = CARTESIAN_POINT ( 'NONE',  ( 2.624999999999998668, -29.08333333333333215, -4.546633369868303021 ) ) ;
#629 = CARTESIAN_POINT ( 'NONE',  ( 3.712013335537174572E-16, -26.96875000068279249, -6.062177826491070398 ) ) ;
#630 = CARTESIAN_POINT ( 'NONE',  ( -5.385316468750000141, -30.10937499965859843, 0.000000000000000000 ) ) ;
#631 = ORIENTED_EDGE ( 'NONE', *, *, #8631, .T. ) ;
#632 = CARTESIAN_POINT ( 'NONE',  ( 5.385316468749999252, -29.43229166632526983, -3.109213912904138954 ) ) ;
#633 = CARTESIAN_POINT ( 'NONE',  ( 1.431606283892694842, -4.050659073900638951, -3.507514324621434199 ) ) ;
#634 = DIRECTION ( 'NONE',  ( -0.000000000000000000, -1.000000000000000000, -0.000000000000000000 ) ) ;
#635 = CARTESIAN_POINT ( 'NONE',  ( 1.975475456537005874E-15, -28.68749999999999645, 5.249999999999999112 ) ) ;
#636 = CIRCLE ( 'NONE', #3913, 5.250000000000000000 ) ;
#637 = DIRECTION ( 'NONE',  ( -0.000000000000000000, -1.000000000000000000, -0.000000000000000000 ) ) ;
#638 = CARTESIAN_POINT ( 'NONE',  ( 6.972266317189433020E-16, -27.71875000068279604, -5.250000000000000000 ) ) ;
#639 = CARTESIAN_POINT ( 'NONE',  ( 5.114683531249999859, -28.83854166700806587, -2.952963913586932776 ) ) ;
#640 = CARTESIAN_POINT ( 'NONE',  ( 0.000000000000000000, -9.000000000000001776, 0.000000000000000000 ) ) ;
#641 = DIRECTION ( 'NONE',  ( 0.000000000000000000, 1.000000000000000000, 0.000000000000000000 ) ) ;
#642 = CARTESIAN_POINT ( 'NONE',  ( -2.134148098076978251, -5.249340926099361759, 2.108492589042307408 ) ) ;
#643 = CARTESIAN_POINT ( 'NONE',  ( 7.041719095097280880E-16, -9.999999999999998224, -5.750000000000000000 ) ) ;
#644 = CARTESIAN_POINT ( 'NONE',  ( 5.385316468750000141, -29.95312499965859843, -6.595110575850215044E-16 ) ) ;
#645 = EDGE_CURVE ( 'NONE', #5282, #1598, #1067, .T. ) ;
#646 = CARTESIAN_POINT ( 'NONE',  ( -1.674995433905516196, -4.250659073900640017, -3.992485675378566690 ) ) ;
#647 = AXIS2_PLACEMENT_3D ( 'NONE', #4691, #1868, #7487 ) ;
#648 = LINE ( 'NONE', #6317, #9109 ) ;
#649 = SURFACE_SIDE_STYLE ('',( #42 ) ) ;
#650 = CARTESIAN_POINT ( 'NONE',  ( -2.351851292788933456, -1.491716277578878685E-16, 2.391493231060961566 ) ) ;
#651 = VECTOR ( 'NONE', #2655, 1000.000000000000000 ) ;
#652 = EDGE_CURVE ( 'NONE', #8139, #3081, #2009, .T. ) ;
#653 = ORIENTED_EDGE ( 'NONE', *, *, #4489, .T. ) ;
#654 =( LENGTH_UNIT ( ) NAMED_UNIT ( * ) SI_UNIT ( .MILLI., .METRE. ) );
#655 = CARTESIAN_POINT ( 'NONE',  ( 5.250000000000000000, -29.37500000000000000, -6.429395695523604153E-16 ) ) ;
#656 = ORIENTED_EDGE ( 'NONE', *, *, #6309, .F. ) ;
#657 = CARTESIAN_POINT ( 'NONE',  ( 3.616337804771879580E-16, -28.04687500034139802, -5.905927827173866440 ) ) ;
#658 = CARTESIAN_POINT ( 'NONE',  ( 2.108492589042307408, -7.249340926099360871, 2.134148098076978251 ) ) ;
#659 = CARTESIAN_POINT ( 'NONE',  ( 5.114683531250000748, -27.17187500034139802, 0.000000000000000000 ) ) ;
#660 = CARTESIAN_POINT ( 'NONE',  ( 2.161402558328724325E-14, -29.31250000000000000, -5.250000000000000000 ) ) ;
#661 = CARTESIAN_POINT ( 'NONE',  ( 5.114683531250000748, -28.92187500034139802, 0.000000000000000000 ) ) ;
#662 = CARTESIAN_POINT ( 'NONE',  ( 5.114683531250000748, -28.17187500034139447, 0.000000000000000000 ) ) ;
#663 = CARTESIAN_POINT ( 'NONE',  ( -5.250000000000000000, -29.25000000000000000, 0.000000000000000000 ) ) ;
#664 = CARTESIAN_POINT ( 'NONE',  ( 5.250000000000000000, -29.79166666598387181, -3.031088913245536531 ) ) ;
#665 = CARTESIAN_POINT ( 'NONE',  ( 0.000000000000000000, -27.00000000000000000, -5.250000000000000000 ) ) ;
#666 = CARTESIAN_POINT ( 'NONE',  ( 0.000000000000000000, 76.00000000000000000, -2.499999999999999556 ) ) ;
#667 = CARTESIAN_POINT ( 'NONE',  ( -1.467888652719046449, -0.5493409260993611376, 3.492485675378536047 ) ) ;
#668 = CARTESIAN_POINT ( 'NONE',  ( 3.507514324621465285, -4.349340926099361404, -1.431606283892619125 ) ) ;
#669 = ORIENTED_EDGE ( 'NONE', *, *, #756, .T. ) ;
#670 = CARTESIAN_POINT ( 'NONE',  ( -6.972266317189433020E-16, -29.06249999999999645, -5.250000000000000000 ) ) ;
#671 = CARTESIAN_POINT ( 'NONE',  ( 3.616337804771879580E-16, -29.29687500034139447, -5.905927827173866440 ) ) ;
#672 = EDGE_CURVE ( 'NONE', #8760, #977, #1244, .T. ) ;
#673 = ORIENTED_EDGE ( 'NONE', *, *, #5568, .T. ) ;
#674 = CARTESIAN_POINT ( 'NONE',  ( 5.385316468750001029, -29.22395833299193413, 3.109213912904134958 ) ) ;
#675 = CARTESIAN_POINT ( 'NONE',  ( -1.431606283892693066, -4.850659073900638774, 3.507514324621434199 ) ) ;
#676 = PLANE ( 'NONE',  #2520 ) ;
#677 = ORIENTED_EDGE ( 'NONE', *, *, #5454, .F. ) ;
#678 = CARTESIAN_POINT ( 'NONE',  ( -1.000000000000000000, -20.00000000000000000, 1.118033988749894680 ) ) ;
#679 = FACE_OUTER_BOUND ( 'NONE', #5811, .T. ) ;
#680 = CARTESIAN_POINT ( 'NONE',  ( 1.406733260263394625, -27.72991455036742536, -5.250000000000000000 ) ) ;
#681 = CARTESIAN_POINT ( 'NONE',  ( -5.114683531250000748, -28.71354166700806587, 2.952963913586931888 ) ) ;
#682 = CARTESIAN_POINT ( 'NONE',  ( -9.180150650966086169E-15, -28.37499999931720041, 5.250000000000000000 ) ) ;
#683 = CARTESIAN_POINT ( 'NONE',  ( -5.249999999999999112, -28.92708333401613174, -3.031088913245536975 ) ) ;
#684 = CARTESIAN_POINT ( 'NONE',  ( -2.134148098076978251, -2.049340926099361138, 2.108492589042307408 ) ) ;
#685 =( BOUNDED_CURVE ( )  B_SPLINE_CURVE ( 2, ( #2269, #6592, #5982, #172, #7986, #7947, #4410, #865, #3715 ),
 .UNSPECIFIED., .F., .F. ) 
 B_SPLINE_CURVE_WITH_KNOTS ( ( 3, 2, 2, 2, 3 ),
 ( 0.7291666666666667407, 0.7361111111111111605, 0.7500000000000000000, 0.7638888888888888395, 0.7708333333333333703 ),
 .UNSPECIFIED. ) 
 CURVE ( )  GEOMETRIC_REPRESENTATION_ITEM ( )  RATIONAL_B_SPLINE_CURVE ( ( 0.9330127018922192983, 0.9330127018922198534, 1.000000000000000000, 0.8660254037844387076, 1.000000000000000000, 0.8660254037844387076, 1.000000000000000000, 0.9330127018922187432, 0.9330127018922192983 ) ) 
 REPRESENTATION_ITEM ( '' )  );
#686 = DIRECTION ( 'NONE',  ( 0.000000000000000000, -1.000000000000000000, 0.000000000000000000 ) ) ;
#687 = CARTESIAN_POINT ( 'NONE',  ( -2.692658234375000514, -29.61979166632526983, -4.663820869356205989 ) ) ;
#688 = CARTESIAN_POINT ( 'NONE',  ( -0.01814118441313417734, -2.550659073900638951, -4.000000000000000000 ) ) ;
#689 = CARTESIAN_POINT ( 'NONE',  ( 3.061616997868382648E-16, 76.00000000000000000, 2.499999999999999556 ) ) ;
#690 = DIRECTION ( 'NONE',  ( 0.000000000000000000, 0.000000000000000000, 1.000000000000000000 ) ) ;
#691 = PRODUCT ( 'cap', 'cap', '', ( #8871 ) ) ;
#692 = ORIENTED_EDGE ( 'NONE', *, *, #6725, .T. ) ;
#693 =( NAMED_UNIT ( * ) PLANE_ANGLE_UNIT ( ) SI_UNIT ( $, .RADIAN. ) );
#694 = CARTESIAN_POINT ( 'NONE',  ( 5.250000000000000888, -29.39583333333332860, 3.031088913245532979 ) ) ;
#695 = CARTESIAN_POINT ( 'NONE',  ( -5.114683531250001636, -28.21354166700806587, 2.952963913586931444 ) ) ;
#696 = CARTESIAN_POINT ( 'NONE',  ( 0.01814118441320878086, -6.249340926099361759, -3.000000000000000444 ) ) ;
#697 = CARTESIAN_POINT ( 'NONE',  ( 5.250000000000000000, -29.72916666666666430, -3.031088913245534755 ) ) ;
#698 = EDGE_CURVE ( 'NONE', #4680, #6430, #9079, .T. ) ;
#699 =( GEOMETRIC_REPRESENTATION_CONTEXT ( 3 ) GLOBAL_UNCERTAINTY_ASSIGNED_CONTEXT ( ( #120 ) ) GLOBAL_UNIT_ASSIGNED_CONTEXT ( ( #327, #6002, #8152 ) ) REPRESENTATION_CONTEXT ( 'NONE', 'WORKASPACE' ) );
#700 = CARTESIAN_POINT ( 'NONE',  ( 3.616337804771879580E-16, -29.85937500034140157, -5.905927827173866440 ) ) ;
#701 = CARTESIAN_POINT ( 'NONE',  ( -2.557341765624999042, -27.58854166700806587, -4.429445870380400052 ) ) ;
#702 = DIRECTION ( 'NONE',  ( 0.000000000000000000, 0.000000000000000000, -1.000000000000000000 ) ) ;
#703 = CARTESIAN_POINT ( 'NONE',  ( 1.113604000661152470E-15, -28.87499999931720396, 6.062177826491070398 ) ) ;
#704 = CARTESIAN_POINT ( 'NONE',  ( 0.000000000000000000, -28.00000000000000000, -2.750000000000000000 ) ) ;
#705 = CARTESIAN_POINT ( 'NONE',  ( -2.019217148918400095, -3.217773791669851107E-17, 2.923265991829747446 ) ) ;
#706 = CARTESIAN_POINT ( 'NONE',  ( -2.692658234374996518, -30.06770833299193413, 4.663820869356208654 ) ) ;
#707 = CARTESIAN_POINT ( 'NONE',  ( -3.492485675378536047, -6.549340926099363358, -1.467888652719048670 ) ) ;
#708 = CARTESIAN_POINT ( 'NONE',  ( -0.01814118441321365544, -3.849340926099361404, 3.500000000000000000 ) ) ;
#709 = EDGE_CURVE ( 'NONE', #2565, #1880, #9113, .T. ) ;
#710 = ORIENTED_EDGE ( 'NONE', *, *, #1444, .T. ) ;
#711 = CYLINDRICAL_SURFACE ( 'NONE', #5192, 1.749999999999999778 ) ;
#712 = CARTESIAN_POINT ( 'NONE',  ( -5.250000000000000000, -27.17708333401612819, -3.031088913245536531 ) ) ;
#713 = ADVANCED_FACE ( 'NONE', ( #520 ), #7635, .F. ) ;
#714 = ORIENTED_EDGE ( 'NONE', *, *, #709, .T. ) ;
#715 = ORIENTED_EDGE ( 'NONE', *, *, #4351, .T. ) ;
#716 = CARTESIAN_POINT ( 'NONE',  ( -3.807688866302469071E-16, -29.89062499965859843, -6.218427825808274356 ) ) ;
#717 = CARTESIAN_POINT ( 'NONE',  ( -1.467888652718973619, -5.850659073900639662, -3.492485675378565801 ) ) ;
#718 = LINE ( 'NONE', #5695, #7261 ) ;
#719 = AXIS2_PLACEMENT_3D ( 'NONE', #7347, #8874, #4420 ) ;
#720 = ORIENTED_EDGE ( 'NONE', *, *, #7534, .F. ) ;
#721 = DIRECTION ( 'NONE',  ( -0.000000000000000000, -0.000000000000000000, 1.000000000000000000 ) ) ;
#722 = DIRECTION ( 'NONE',  ( 0.000000000000000000, 0.000000000000000000, -1.000000000000000000 ) ) ;
#723 = DIRECTION ( 'NONE',  ( 1.000000000000000000, 0.000000000000000000, 0.000000000000000000 ) ) ;
#724 = AXIS2_PLACEMENT_3D ( 'NONE', #8229, #4642, #1153 ) ;
#725 = CARTESIAN_POINT ( 'NONE',  ( 2.557341765624996821, -28.90104166700806587, 4.429445870380401828 ) ) ;
#726 = FACE_OUTER_BOUND ( 'NONE', #1560, .T. ) ;
#727 = CARTESIAN_POINT ( 'NONE',  ( 1.185285273922203525E-14, -28.96875000068279959, -5.250000000000000000 ) ) ;
#728 = CARTESIAN_POINT ( 'NONE',  ( 3.007514324621463508, -2.749340926099361759, -1.224499502706076770 ) ) ;
#729 = CARTESIAN_POINT ( 'NONE',  ( 5.204748896376250699E-16, -9.000000000000001776, -4.250000000000000000 ) ) ;
#730 = CARTESIAN_POINT ( 'NONE',  ( -5.385316468750001029, -28.38020833299193058, -3.109213912904136734 ) ) ;
#731 = CARTESIAN_POINT ( 'NONE',  ( 1.638713065079247855, -0.8506590739006385515, -4.007514324621431534 ) ) ;
#732 = VECTOR ( 'NONE', #6064, 1000.000000000000000 ) ;
#733 = DIRECTION ( 'NONE',  ( -0.000000000000000000, -1.000000000000000000, -0.000000000000000000 ) ) ;
#734 = DIRECTION ( 'NONE',  ( 1.067350013832299517E-17, -0.9961946980917455452, 0.08715574274765836016 ) ) ;
#735 = SHAPE_REPRESENTATION ( 'MAS-161', ( #6650, #7552, #3536, #4130, #8732, #264, #6206, #8298, #4727, #2658 ), #1446 ) ;
#736 = ORIENTED_EDGE ( 'NONE', *, *, #3059, .T. ) ;
#737 = CARTESIAN_POINT ( 'NONE',  ( -5.250000000000000000, -29.25000000000000000, 0.000000000000000000 ) ) ;
#738 = VERTEX_POINT ( 'NONE', #4144 ) ;
#739 = CARTESIAN_POINT ( 'NONE',  ( -1.406733260263393070, -27.30133545031536357, -5.250000000000000888 ) ) ;
#740 = CARTESIAN_POINT ( 'NONE',  ( -1.260781871532431708, -1.050659073900639617, -2.992485675378564469 ) ) ;
#741 = PRODUCT_DEFINITION ( 'UNKNOWN', '', #1604, #6719 ) ;
#742 = CONICAL_SURFACE ( 'NONE', #6530, 2.000000000000000000, 0.06981317007977333455 ) ;
#743 = EDGE_LOOP ( 'NONE', ( #7927, #7894 ) ) ;
#744 = CARTESIAN_POINT ( 'NONE',  ( -1.113604000661152470E-15, -29.81250000000000000, 6.062177826491070398 ) ) ;
#745 = DIRECTION ( 'NONE',  ( 0.000000000000000000, 0.000000000000000000, 1.000000000000000000 ) ) ;
#746 = CARTESIAN_POINT ( 'NONE',  ( -2.557341765625002594, -28.50520833367473017, 4.429445870380399164 ) ) ;
#747 = AXIS2_PLACEMENT_3D ( 'NONE', #6440, #4909, #7757 ) ;
#748 =( NAMED_UNIT ( * ) PLANE_ANGLE_UNIT ( ) SI_UNIT ( $, .RADIAN. ) );
#749 = CARTESIAN_POINT ( 'NONE',  ( -2.557341765624999042, -28.08854166700806587, -4.429445870380400052 ) ) ;
#750 = CARTESIAN_POINT ( 'NONE',  ( 5.250000000000000000, -28.81249999931720396, -6.429395695523604153E-16 ) ) ;
#751 = CARTESIAN_POINT ( 'NONE',  ( 5.250000000000000000, -27.56249999931720396, -6.429395695523604153E-16 ) ) ;
#752 = CARTESIAN_POINT ( 'NONE',  ( 5.249999999999997335, -29.55208333401613885, 3.031088913245538308 ) ) ;
#753 = CARTESIAN_POINT ( 'NONE',  ( 2.300847884672513123E-14, -28.43750000000000000, -5.250000000000000000 ) ) ;
#754 = CARTESIAN_POINT ( 'NONE',  ( 5.114683531249998971, -29.44270833367473372, 2.952963913586936329 ) ) ;
#755 = CARTESIAN_POINT ( 'NONE',  ( 2.487701488670255756, -4.449340926099361937, -2.462045979635577364 ) ) ;
#756 = EDGE_CURVE ( 'NONE', #7705, #8808, #3387, .T. ) ;
#757 = EDGE_LOOP ( 'NONE', ( #8210, #7399, #8601, #6496 ) ) ;
#758 = CARTESIAN_POINT ( 'NONE',  ( -1.467888652718973841, -5.850659073900639662, -3.492485675378565801 ) ) ;
#759 = CARTESIAN_POINT ( 'NONE',  ( -1.406733260263394625, -27.55133545031536713, -5.250000000000000000 ) ) ;
#760 = CARTESIAN_POINT ( 'NONE',  ( -1.084901341431563923E-15, -29.67187500034139802, 5.905927827173866440 ) ) ;
#761 = EDGE_CURVE ( 'NONE', #7091, #2823, #648, .T. ) ;
#762 = ORIENTED_EDGE ( 'NONE', *, *, #2487, .F. ) ;
#763 =( BOUNDED_CURVE ( )  B_SPLINE_CURVE ( 2, ( #6831, #8182, #8914, #7483, #3951, #7577, #6926, #6129, #8961 ),
 .UNSPECIFIED., .F., .T. ) 
 B_SPLINE_CURVE_WITH_KNOTS ( ( 3, 2, 2, 2, 3 ),
 ( 0.3541666666666666297, 0.3611111111111111049, 0.3750000000000000000, 0.3888888888888888951, 0.3958333333333333703 ),
 .UNSPECIFIED. ) 
 CURVE ( )  GEOMETRIC_REPRESENTATION_ITEM ( )  RATIONAL_B_SPLINE_CURVE ( ( 0.9330127018922194093, 0.9330127018922190762, 1.000000000000000000, 0.8660254037844387076, 1.000000000000000000, 0.8660254037844387076, 1.000000000000000000, 0.9330127018922190762, 0.9330127018922194093 ) ) 
 REPRESENTATION_ITEM ( '' )  );
#764 = ORIENTED_EDGE ( 'NONE', *, *, #4966, .T. ) ;
#765 = CARTESIAN_POINT ( 'NONE',  ( 5.385316468750000141, -29.70312499965859843, -6.595110575850215044E-16 ) ) ;
#766 = CARTESIAN_POINT ( 'NONE',  ( -3.992485675378568022, 0.1493409260993615040, 1.674995433905515529 ) ) ;
#767 = CARTESIAN_POINT ( 'NONE',  ( 6.429395695523604153E-16, -27.00000000000000000, 5.250000000000000000 ) ) ;
#768 = EDGE_CURVE ( 'NONE', #2834, #2260, #8516, .T. ) ;
#769 = EDGE_LOOP ( 'NONE', ( #7449, #1488, #232, #2395 ) ) ;
#770 = CARTESIAN_POINT ( 'NONE',  ( -6.972266317189433020E-16, -29.06249999999999645, -5.250000000000000000 ) ) ;
#771 = CARTESIAN_POINT ( 'NONE',  ( 6.429395695523604153E-16, -27.00000000000000000, 5.250000000000000000 ) ) ;
#772 = CARTESIAN_POINT ( 'NONE',  ( 5.250000000000000888, -27.33333333265053611, 3.031088913245533423 ) ) ;
#773 = CARTESIAN_POINT ( 'NONE',  ( 5.114683531249999859, -28.58854166700806232, -2.952963913586932776 ) ) ;
#774 = PLANE ( 'NONE',  #1388 ) ;
#775 = CARTESIAN_POINT ( 'NONE',  ( 2.625000000000000444, -28.98958333401613174, -4.546633369868303021 ) ) ;
#776 = CARTESIAN_POINT ( 'NONE',  ( -2.134148098076978251, -3.649340926099361671, 2.108492589042307408 ) ) ;
#777 = DIRECTION ( 'NONE',  ( 0.000000000000000000, 0.000000000000000000, 1.000000000000000000 ) ) ;
#778 = CARTESIAN_POINT ( 'NONE',  ( -2.692658234375000514, -27.65104166632526628, -4.663820869356205989 ) ) ;
#779 = CARTESIAN_POINT ( 'NONE',  ( -2.841254879263473310, -7.550659073900639839, -2.815599370228907716 ) ) ;
#780 = AXIS2_PLACEMENT_3D ( 'NONE', #6952, #8529, #7794 ) ;
#781 = CARTESIAN_POINT ( 'NONE',  ( 3.061616997868383634E-16, -20.00000000000000000, -2.500000000000000444 ) ) ;
#782 = CARTESIAN_POINT ( 'NONE',  ( 6.972266317189433020E-16, -27.71875000068279604, -5.250000000000000000 ) ) ;
#783 = EDGE_CURVE ( 'NONE', #3636, #7860, #7922, .T. ) ;
#784 = VERTEX_POINT ( 'NONE', #5850 ) ;
#785 = AXIS2_PLACEMENT_3D ( 'NONE', #1263, #6935, #563 ) ;
#786 = CARTESIAN_POINT ( 'NONE',  ( 2.692658234375002735, -27.49479166632526628, 4.663820869356205101 ) ) ;
#787 = COLOUR_RGB ( '',0.8941176470588234615, 0.8941176470588234615, 0.8941176470588234615 ) ;
#788 = ORIENTED_EDGE ( 'NONE', *, *, #7385, .F. ) ;
#789 = CARTESIAN_POINT ( 'NONE',  ( 0.000000000000000000, 75.00000000000000000, 5.250000000000000000 ) ) ;
#790 = CARTESIAN_POINT ( 'NONE',  ( -1.260781871532431708, -4.250659073900640017, -2.992485675378564469 ) ) ;
#791 = VERTEX_POINT ( 'NONE', #4553 ) ;
#792 = CARTESIAN_POINT ( 'NONE',  ( -5.250000000000000000, -28.64583333333332860, -3.031088913245536531 ) ) ;
#793 = LINE ( 'NONE', #3457, #2596 ) ;
#794 = CIRCLE ( 'NONE', #5842, 5.750000000000000000 ) ;
#795 = CARTESIAN_POINT ( 'NONE',  ( 5.114683531250000748, -27.42187500034139802, 0.000000000000000000 ) ) ;
#796 = CARTESIAN_POINT ( 'NONE',  ( -2.557341765625002594, -27.50520833367473017, 4.429445870380399164 ) ) ;
#797 = CARTESIAN_POINT ( 'NONE',  ( -3.712013335537174572E-16, -29.99999999931720041, -6.062177826491070398 ) ) ;
#798 = CARTESIAN_POINT ( 'NONE',  ( -1.975475456537005874E-15, -29.59375000068279249, 5.249999999999999112 ) ) ;
#799 = DIRECTION ( 'NONE',  ( 0.000000000000000000, 1.000000000000000000, 0.000000000000000000 ) ) ;
#800 = CARTESIAN_POINT ( 'NONE',  ( -5.250000000000000000, -27.75000000000000000, 0.000000000000000000 ) ) ;
#801 = CARTESIAN_POINT ( 'NONE',  ( -5.114683531250000748, -29.77604166700806232, 2.952963913586931888 ) ) ;
#802 = CARTESIAN_POINT ( 'NONE',  ( 2.487701488670255756, -7.649340926099361226, -2.462045979635577364 ) ) ;
#803 = VERTEX_POINT ( 'NONE', #1062 ) ;
#804 = CARTESIAN_POINT ( 'NONE',  ( 1.431606283892694620, -5.650659073900638596, -3.507514324621433754 ) ) ;
#805 = DIRECTION ( 'NONE',  ( 0.000000000000000000, 1.000000000000000000, 0.000000000000000000 ) ) ;
#806 = CARTESIAN_POINT ( 'NONE',  ( 5.114683531249999859, -27.83854166700806587, -2.952963913586932776 ) ) ;
#807 = EDGE_LOOP ( 'NONE', ( #1458, #4944, #5003, #5759 ) ) ;
#808 = EDGE_LOOP ( 'NONE', ( #7978, #931, #7565, #1484 ) ) ;
#809 = CARTESIAN_POINT ( 'NONE',  ( 5.249999999999999112, -29.60416666666666785, -3.031088913245536975 ) ) ;
#810 = LINE ( 'NONE', #5926, #186 ) ;
#811 = CARTESIAN_POINT ( 'NONE',  ( 2.841254879263473310, -6.750659073900638241, 2.815599370228907272 ) ) ;
#812 = CARTESIAN_POINT ( 'NONE',  ( 5.250000000000000888, -29.33333333265053611, 3.031088913245533423 ) ) ;
#813 = VERTEX_POINT ( 'NONE', #6729 ) ;
#814 = EDGE_CURVE ( 'NONE', #4395, #3226, #6461, .T. ) ;
#815 = CARTESIAN_POINT ( 'NONE',  ( -1.975475456537005874E-15, -29.34375000068279249, 5.250000000000000000 ) ) ;
#816 = CARTESIAN_POINT ( 'NONE',  ( -5.250000000000000000, -29.42708333401613174, -3.031088913245536531 ) ) ;
#817 =( BOUNDED_SURFACE ( )  B_SPLINE_SURFACE ( 1, 2, ( 
 ( #3707, #7233, #6674, #2454, #3848, #5280, #6532, #7376, #858, #2968, #5840, #8125, #5090, #256, #4446, #2262, #8679, #816, #304, #3157, #5137, #7284, #1562, #4359, #3108, #4403, #7192, #3757, #3657, #2403, #6585, #5932, #2356, #214, #4499, #6483, #118, #5185, #3066, #8773, #5791, #8633, #5885, #8723, #956, #1658, #8028, #7331, #5232, #8077, #1706, #6629, #4544, #8998, #1196, #3898, #3343, #1945, #2646, #6717, #8222, #1242, #4040, #5518, #7427, #6872, #6821, #3991, #398, #544, #1855, #6172, #4084, #5372, #3245, #6069, #2551, #2498, #7519, #7617, #3385, #1148, #8314, #8859, #6770, #1052, #4682, #5322, #351, #448, #1754, #6919, #7473, #8905, #3294, #4773, #498, #6217, #9046, #3201, #6122, #4590, #8951, #5467, #2691, #6022, #8176, #1899, #2602, #5419, #1802, #4635, #1103, #3943, #8268, #4726, #7568, #588, #3516, #4255, #3604, #1284, #5560, #7089, #2116, #712, #7799, #4215, #8361, #2735, #8446, #6429, #65, #4301, #6300, #629, #5601, #2162, #9137, #3472, #4899, #7662, #6957, #1456, #9092 ),
 ( #8534, #3432, #4818, #7751, #3560, #8495, #9176, #2781, #2915, #760, #7139, #4982, #6383, #4855, #2071, #1415, #1987, #8405, #4123, #6261, #2032, #7838, #6340, #7004, #7701, #5689, #1327, #671, #4170, #1373, #7047, #2826, #5646, #4941, #21, #2869, #6522, #294, #5223, #2301, #3749, #7223, #948, #3007, #1597, #7972, #4394, #1504, #8018, #848, #1553, #3098, #3696, #5028, #8714, #2394, #5076, #3649, #157, #1650, #3795, #8669, #4535, #2958, #4488, #5732, #5830, #990, #5125, #6619, #7321, #7930, #4437, #7273, #246, #5920, #108, #5779, #900, #6571, #3836, #8066, #8763, #6662, #8577, #1696, #7366, #205, #3056, #8622, #5876, #2205, #2345, #2252, #7885, #4347, #7183, #806, #5175, #6473, #8850, #1743, #6012, #1229, #3889, #8257, #3235, #1037, #2489, #8807, #8986, #2634, #3933, #4624, #4760, #7555, #3280, #2589, #3978, #5312, #8208, #1842, #1138, #1792, #1091, #2444, #1932, #6760, #4580, #1181, #5407, #5269, #4715, #3328, #4025, #8115, #386, #5455, #1890, #6907, #7415, #6860, #4671, #5361, #7464 ) ),
 .UNSPECIFIED., .F., .F., .F. ) 
 B_SPLINE_SURFACE_WITH_KNOTS ( ( 2, 2 ),
 ( 3, 2, 2, 2, 2, 2, 2, 2, 2, 2, 2, 2, 2, 2, 2, 2, 2, 2, 2, 2, 2, 2, 2, 2, 2, 2, 2, 2, 2, 2, 2, 2, 2, 2, 2, 2, 2, 2, 2, 2, 2, 2, 2, 2, 2, 2, 2, 2, 2, 2, 2, 2, 2, 2, 2, 2, 2, 2, 2, 2, 2, 2, 2, 2, 2, 2, 2, 2, 2, 2, 2, 2, 3 ),
 ( 0.000000000000000000, 1.000000000000000000 ),
 ( 0.000000000000000000, 0.01388888888888888812, 0.02777777777777777624, 0.04166666666666666435, 0.05555555555555555247, 0.06944444444444444753, 0.08333333333333332871, 0.09722222222222222376, 0.1111111111111111049, 0.1250000000000000000, 0.1388888888888888951, 0.1527777777777777901, 0.1666666666666666574, 0.1805555555555555525, 0.1944444444444444475, 0.2083333333333333426, 0.2222222222222222099, 0.2361111111111111049, 0.2500000000000000000, 0.2638888888888888951, 0.2777777777777777901, 0.2916666666666666852, 0.3055555555555555802, 0.3194444444444444198, 0.3333333333333333148, 0.3472222222222222099, 0.3611111111111111049, 0.3750000000000000000, 0.3888888888888888951, 0.4027777777777777901, 0.4166666666666666852, 0.4305555555555555802, 0.4444444444444444198, 0.4583333333333333148, 0.4722222222222222099, 0.4861111111111111049, 0.5000000000000000000, 0.5138888888888888395, 0.5277777777777777901, 0.5416666666666666297, 0.5555555555555555802, 0.5694444444444444198, 0.5833333333333333703, 0.5972222222222222099, 0.6111111111111111605, 0.6250000000000000000, 0.6388888888888888395, 0.6527777777777777901, 0.6666666666666666297, 0.6805555555555555802, 0.6944444444444444198, 0.7083333333333333703, 0.7222222222222222099, 0.7361111111111111605, 0.7500000000000000000, 0.7638888888888888395, 0.7777777777777777901, 0.7916666666666666297, 0.8055555555555555802, 0.8194444444444444198, 0.8333333333333333703, 0.8472222222222222099, 0.8611111111111111605, 0.8750000000000000000, 0.8888888888888888395, 0.9027777777777777901, 0.9166666666666666297, 0.9305555555555555802, 0.9444444444444444198, 0.9583333333333333703, 0.9722222222222222099, 0.9861111111111111605, 1.000000000000000000 ),
 .UNSPECIFIED. ) 
 GEOMETRIC_REPRESENTATION_ITEM ( )  RATIONAL_B_SPLINE_SURFACE ( (
 ( 1.000000000000000000, 0.8660254037844387076, 1.000000000000000000, 0.8660254037844387076, 1.000000000000000000, 0.8660254037844387076, 1.000000000000000000, 0.8660254037844387076, 1.000000000000000000, 0.8660254037844387076, 1.000000000000000000, 0.8660254037844387076, 1.000000000000000000, 0.8660254037844387076, 1.000000000000000000, 0.8660254037844387076, 1.000000000000000000, 0.8660254037844387076, 1.000000000000000000, 0.8660254037844387076, 1.000000000000000000, 0.8660254037844387076, 1.000000000000000000, 0.8660254037844387076, 1.000000000000000000, 0.8660254037844387076, 1.000000000000000000, 0.8660254037844387076, 1.000000000000000000, 0.8660254037844387076, 1.000000000000000000, 0.8660254037844387076, 1.000000000000000000, 0.8660254037844387076, 1.000000000000000000, 0.8660254037844387076, 1.000000000000000000, 0.8660254037844387076, 1.000000000000000000, 0.8660254037844387076, 1.000000000000000000, 0.8660254037844387076, 1.000000000000000000, 0.8660254037844387076, 1.000000000000000000, 0.8660254037844387076, 1.000000000000000000, 0.8660254037844387076, 1.000000000000000000, 0.8660254037844387076, 1.000000000000000000, 0.8660254037844387076, 1.000000000000000000, 0.8660254037844387076, 1.000000000000000000, 0.8660254037844387076, 1.000000000000000000, 0.8660254037844387076, 1.000000000000000000, 0.8660254037844387076, 1.000000000000000000, 0.8660254037844387076, 1.000000000000000000, 0.8660254037844387076, 1.000000000000000000, 0.8660254037844387076, 1.000000000000000000, 0.8660254037844387076, 1.000000000000000000, 0.8660254037844387076, 1.000000000000000000, 0.8660254037844387076, 1.000000000000000000, 0.8660254037844387076, 1.000000000000000000, 0.8660254037844387076, 1.000000000000000000, 0.8660254037844387076, 1.000000000000000000, 0.8660254037844387076, 1.000000000000000000, 0.8660254037844387076, 1.000000000000000000, 0.8660254037844387076, 1.000000000000000000, 0.8660254037844387076, 1.000000000000000000, 0.8660254037844387076, 1.000000000000000000, 0.8660254037844387076, 1.000000000000000000, 0.8660254037844387076, 1.000000000000000000, 0.8660254037844387076, 1.000000000000000000, 0.8660254037844387076, 1.000000000000000000, 0.8660254037844387076, 1.000000000000000000, 0.8660254037844387076, 1.000000000000000000, 0.8660254037844387076, 1.000000000000000000, 0.8660254037844387076, 1.000000000000000000, 0.8660254037844387076, 1.000000000000000000, 0.8660254037844387076, 1.000000000000000000, 0.8660254037844387076, 1.000000000000000000, 0.8660254037844387076, 1.000000000000000000, 0.8660254037844387076, 1.000000000000000000, 0.8660254037844387076, 1.000000000000000000, 0.8660254037844387076, 1.000000000000000000, 0.8660254037844387076, 1.000000000000000000, 0.8660254037844387076, 1.000000000000000000, 0.8660254037844387076, 1.000000000000000000, 0.8660254037844387076, 1.000000000000000000, 0.8660254037844387076, 1.000000000000000000, 0.8660254037844387076, 1.000000000000000000, 0.8660254037844387076, 1.000000000000000000, 0.8660254037844387076, 1.000000000000000000, 0.8660254037844387076, 1.000000000000000000, 0.8660254037844387076, 1.000000000000000000, 0.8660254037844387076, 1.000000000000000000, 0.8660254037844387076, 1.000000000000000000, 0.8660254037844387076, 1.000000000000000000),
 ( 1.000000000000000000, 0.8660254037844387076, 1.000000000000000000, 0.8660254037844387076, 1.000000000000000000, 0.8660254037844387076, 1.000000000000000000, 0.8660254037844387076, 1.000000000000000000, 0.8660254037844387076, 1.000000000000000000, 0.8660254037844387076, 1.000000000000000000, 0.8660254037844387076, 1.000000000000000000, 0.8660254037844387076, 1.000000000000000000, 0.8660254037844387076, 1.000000000000000000, 0.8660254037844387076, 1.000000000000000000, 0.8660254037844387076, 1.000000000000000000, 0.8660254037844387076, 1.000000000000000000, 0.8660254037844387076, 1.000000000000000000, 0.8660254037844387076, 1.000000000000000000, 0.8660254037844387076, 1.000000000000000000, 0.8660254037844387076, 1.000000000000000000, 0.8660254037844387076, 1.000000000000000000, 0.8660254037844387076, 1.000000000000000000, 0.8660254037844387076, 1.000000000000000000, 0.8660254037844387076, 1.000000000000000000, 0.8660254037844387076, 1.000000000000000000, 0.8660254037844387076, 1.000000000000000000, 0.8660254037844387076, 1.000000000000000000, 0.8660254037844387076, 1.000000000000000000, 0.8660254037844387076, 1.000000000000000000, 0.8660254037844387076, 1.000000000000000000, 0.8660254037844387076, 1.000000000000000000, 0.8660254037844387076, 1.000000000000000000, 0.8660254037844387076, 1.000000000000000000, 0.8660254037844387076, 1.000000000000000000, 0.8660254037844387076, 1.000000000000000000, 0.8660254037844387076, 1.000000000000000000, 0.8660254037844387076, 1.000000000000000000, 0.8660254037844387076, 1.000000000000000000, 0.8660254037844387076, 1.000000000000000000, 0.8660254037844387076, 1.000000000000000000, 0.8660254037844387076, 1.000000000000000000, 0.8660254037844387076, 1.000000000000000000, 0.8660254037844387076, 1.000000000000000000, 0.8660254037844387076, 1.000000000000000000, 0.8660254037844387076, 1.000000000000000000, 0.8660254037844387076, 1.000000000000000000, 0.8660254037844387076, 1.000000000000000000, 0.8660254037844387076, 1.000000000000000000, 0.8660254037844387076, 1.000000000000000000, 0.8660254037844387076, 1.000000000000000000, 0.8660254037844387076, 1.000000000000000000, 0.8660254037844387076, 1.000000000000000000, 0.8660254037844387076, 1.000000000000000000, 0.8660254037844387076, 1.000000000000000000, 0.8660254037844387076, 1.000000000000000000, 0.8660254037844387076, 1.000000000000000000, 0.8660254037844387076, 1.000000000000000000, 0.8660254037844387076, 1.000000000000000000, 0.8660254037844387076, 1.000000000000000000, 0.8660254037844387076, 1.000000000000000000, 0.8660254037844387076, 1.000000000000000000, 0.8660254037844387076, 1.000000000000000000, 0.8660254037844387076, 1.000000000000000000, 0.8660254037844387076, 1.000000000000000000, 0.8660254037844387076, 1.000000000000000000, 0.8660254037844387076, 1.000000000000000000, 0.8660254037844387076, 1.000000000000000000, 0.8660254037844387076, 1.000000000000000000, 0.8660254037844387076, 1.000000000000000000, 0.8660254037844387076, 1.000000000000000000, 0.8660254037844387076, 1.000000000000000000, 0.8660254037844387076, 1.000000000000000000, 0.8660254037844387076, 1.000000000000000000, 0.8660254037844387076, 1.000000000000000000, 0.8660254037844387076, 1.000000000000000000, 0.8660254037844387076, 1.000000000000000000) ) ) 
 REPRESENTATION_ITEM ( '' )  SURFACE ( )  );
#818 = CARTESIAN_POINT ( 'NONE',  ( -5.385316468750000141, -27.10937499965860198, 0.000000000000000000 ) ) ;
#819 = CARTESIAN_POINT ( 'NONE',  ( 5.114683531250000748, -26.85937500034139802, 0.000000000000000000 ) ) ;
#820 = FACE_OUTER_BOUND ( 'NONE', #3345, .T. ) ;
#821 = CARTESIAN_POINT ( 'NONE',  ( 2.692658234374998738, -27.16145833299193413, -4.663820869356206877 ) ) ;
#822 = CARTESIAN_POINT ( 'NONE',  ( 3.007514324621463508, -4.349340926099361404, -1.224499502706076770 ) ) ;
#823 = CARTESIAN_POINT ( 'NONE',  ( 0.000000000000000000, -27.00000000000000000, 0.000000000000000000 ) ) ;
#824 = CARTESIAN_POINT ( 'NONE',  ( 2.692658234375002735, -28.52604166632526628, 4.663820869356205101 ) ) ;
#825 = CARTESIAN_POINT ( 'NONE',  ( 0.01814118441321938349, -4.649340926099361226, -4.000000000000000000 ) ) ;
#826 = ADVANCED_FACE ( 'NONE', ( #3906 ), #1011, .T. ) ;
#827 = CARTESIAN_POINT ( 'NONE',  ( 0.000000000000000000, 75.00000000000000000, 0.000000000000000000 ) ) ;
#828 = CARTESIAN_POINT ( 'NONE',  ( -1.406733260263385521, -27.82366454968462932, 5.250000000000006217 ) ) ;
#829 = CARTESIAN_POINT ( 'NONE',  ( 2.624999999999998668, -29.02083333265053611, -4.546633369868303021 ) ) ;
#830 = EDGE_LOOP ( 'NONE', ( #2328, #67 ) ) ;
#831 = CARTESIAN_POINT ( 'NONE',  ( 2.625000000000002220, -29.66666666666666785, 4.546633369868302132 ) ) ;
#832 = ORIENTED_EDGE ( 'NONE', *, *, #1444, .F. ) ;
#833 = CARTESIAN_POINT ( 'NONE',  ( 0.000000000000000000, -30.00000000000000000, 0.000000000000000000 ) ) ;
#834 = CARTESIAN_POINT ( 'NONE',  ( 2.992485675378565357, -7.050659073900639839, -1.260781871532430376 ) ) ;
#835 = ORIENTED_EDGE ( 'NONE', *, *, #8338, .F. ) ;
#836 = CARTESIAN_POINT ( 'NONE',  ( -5.250000000000000000, -29.39583333333332860, -3.031088913245536531 ) ) ;
#837 = CARTESIAN_POINT ( 'NONE',  ( 3.616337804771879580E-16, -27.35937500034139802, -5.905927827173866440 ) ) ;
#838 = CARTESIAN_POINT ( 'NONE',  ( -5.114683531250000748, -27.79687500034139802, -6.263680815196995234E-16 ) ) ;
#839 = CARTESIAN_POINT ( 'NONE',  ( -5.249999999999999112, -30.16666666598386470, 3.031088913245538308 ) ) ;
#840 = CARTESIAN_POINT ( 'NONE',  ( 3.500000000000000000, -2.649340926099361226, 0.01814118441321387054 ) ) ;
#841 = LINE ( 'NONE', #941, #8467 ) ;
#842 = CARTESIAN_POINT ( 'NONE',  ( -2.624999999999996891, -28.20833333333333215, 4.546633369868304797 ) ) ;
#843 = CARTESIAN_POINT ( 'NONE',  ( 0.000000000000000000, -29.87813065659485190, -5.257453848358681014 ) ) ;
#844 = SURFACE_SIDE_STYLE ('',( #2821 ) ) ;
#845 = VERTEX_POINT ( 'NONE', #3118 ) ;
#846 = CARTESIAN_POINT ( 'NONE',  ( 5.250000000000000888, -27.14583333333332860, 3.031088913245533423 ) ) ;
#847 = DIRECTION ( 'NONE',  ( 0.000000000000000000, 1.000000000000000000, 0.000000000000000000 ) ) ;
#848 = CARTESIAN_POINT ( 'NONE',  ( 5.114683531249999859, -28.83854166700806587, -2.952963913586932776 ) ) ;
#849 = VERTEX_POINT ( 'NONE', #7295 ) ;
#850 = MECHANICAL_DESIGN_GEOMETRIC_PRESENTATION_REPRESENTATION (  '', ( #4576 ), #5468 ) ;
#851 = EDGE_CURVE ( 'NONE', #8796, #3220, #8383, .T. ) ;
#852 = ORIENTED_EDGE ( 'NONE', *, *, #1586, .F. ) ;
#853 = CARTESIAN_POINT ( 'NONE',  ( 2.624999999999996891, -26.82291666734946389, 4.546633369868304797 ) ) ;
#854 = CARTESIAN_POINT ( 'NONE',  ( 5.385316468749999252, -27.21354166632526628, -3.109213912904138954 ) ) ;
#855 = CARTESIAN_POINT ( 'NONE',  ( -0.01814118441321889430, -0.6493409260993606713, 4.000000000000000000 ) ) ;
#856 = ORIENTED_EDGE ( 'NONE', *, *, #3685, .T. ) ;
#857 = CARTESIAN_POINT ( 'NONE',  ( 5.249999999999999112, -29.85416666666666785, -3.031088913245536975 ) ) ;
#858 = CARTESIAN_POINT ( 'NONE',  ( -2.625000000000002220, -29.61458333401613174, 4.546633369868302132 ) ) ;
#859 = CARTESIAN_POINT ( 'NONE',  ( -5.385316468750001029, -27.88020833299193413, -3.109213912904136734 ) ) ;
#860 = UNCERTAINTY_MEASURE_WITH_UNIT (LENGTH_MEASURE( 1.000000000000000082E-05 ), #473, 'distance_accuracy_value', 'NONE');
#861 = CARTESIAN_POINT ( 'NONE',  ( 2.557341765625000818, -27.81770833367473017, -4.429445870380400052 ) ) ;
#862 = CARTESIAN_POINT ( 'NONE',  ( -3.500000000000000000, -0.2493409260993610654, -0.01814118441321344033 ) ) ;
#863 = CARTESIAN_POINT ( 'NONE',  ( 5.385316468749999252, -27.18229166632526628, -3.109213912904138954 ) ) ;
#864 = CARTESIAN_POINT ( 'NONE',  ( -0.01814118441314477650, -2.550659073900638951, -3.000000000000000444 ) ) ;
#865 = CARTESIAN_POINT ( 'NONE',  ( -1.406733260263384411, -29.48883544963257464, -5.250000000000006217 ) ) ;
#866 = CARTESIAN_POINT ( 'NONE',  ( 2.815599370228907716, -7.150659073900638596, -2.841254879263473310 ) ) ;
#867 = EDGE_CURVE ( 'NONE', #8201, #5024, #2277, .T. ) ;
#868 = CARTESIAN_POINT ( 'NONE',  ( 5.250000000000000000, -27.56249999931720396, -6.429395695523604153E-16 ) ) ;
#869 = CARTESIAN_POINT ( 'NONE',  ( 5.250000000000000888, -27.64583333333333570, 3.031088913245533423 ) ) ;
#870 = VECTOR ( 'NONE', #6866, 1000.000000000000000 ) ;
#871 = CARTESIAN_POINT ( 'NONE',  ( 3.492485675378535603, -2.549340926099361138, 1.467888652719046672 ) ) ;
#872 = EDGE_CURVE ( 'NONE', #8537, #7146, #935, .T. ) ;
#873 = CARTESIAN_POINT ( 'NONE',  ( 0.000000000000000000, -29.00000000000000355, 0.000000000000000000 ) ) ;
#874 = VERTEX_POINT ( 'NONE', #312 ) ;
#875 = CARTESIAN_POINT ( 'NONE',  ( 0.000000000000000000, 0.000000000000000000, 0.000000000000000000 ) ) ;
#876 = CARTESIAN_POINT ( 'NONE',  ( 2.692658234374998738, -27.91145833299193413, -4.663820869356206877 ) ) ;
#877 = CARTESIAN_POINT ( 'NONE',  ( 2.815599370228847320, -2.449340926099361049, 2.841254879263533262 ) ) ;
#878 = CARTESIAN_POINT ( 'NONE',  ( 3.673940397442060361E-16, 70.00000000000000000, 3.000000000000000444 ) ) ;
#879 = EDGE_LOOP ( 'NONE', ( #5757, #6091 ) ) ;
#880 =( GEOMETRIC_REPRESENTATION_CONTEXT ( 3 ) GLOBAL_UNCERTAINTY_ASSIGNED_CONTEXT ( ( #5144 ) ) GLOBAL_UNIT_ASSIGNED_CONTEXT ( ( #5512, #7423, #9170 ) ) REPRESENTATION_CONTEXT ( 'NONE', 'WORKASPACE' ) );
#881 = CYLINDRICAL_SURFACE ( 'NONE', #3176, 5.250000000000000000 ) ;
#882 = CARTESIAN_POINT ( 'NONE',  ( -2.134148098076932953, -7.550659073900640728, -2.108492589042352705 ) ) ;
#883 = ORIENTED_EDGE ( 'NONE', *, *, #8729, .F. ) ;
#884 = CARTESIAN_POINT ( 'NONE',  ( -5.250000000000000888, -29.10416666666666785, 3.031088913245532979 ) ) ;
#885 = EDGE_CURVE ( 'NONE', #8537, #845, #3165, .T. ) ;
#886 = AXIS2_PLACEMENT_3D ( 'NONE', #6121, #3897, #6716 ) ;
#887 = CARTESIAN_POINT ( 'NONE',  ( -1.084901341431563726E-15, -27.23437500034139802, 5.905927827173866440 ) ) ;
#888 = AXIS2_PLACEMENT_3D ( 'NONE', #4026, #9081, #6861 ) ;
#889 = CARTESIAN_POINT ( 'NONE',  ( -2.625000000000000444, -27.04166666666666430, -4.546633369868303021 ) ) ;
#890 = CIRCLE ( 'NONE', #3281, 5.250000000000000000 ) ;
#891 = CARTESIAN_POINT ( 'NONE',  ( -2.557341765624999042, -29.77604166700806232, -4.429445870380400052 ) ) ;
#892 = CARTESIAN_POINT ( 'NONE',  ( -2.487701488670255312, -3.649340926099361226, 2.462045979635577808 ) ) ;
#893 = CARTESIAN_POINT ( 'NONE',  ( 0.000000000000000000, 79.00000000000001421, 0.000000000000000000 ) ) ;
#894 = CARTESIAN_POINT ( 'NONE',  ( -1.000000000000000000, -30.99987166532831395, 2.582963027349738816 ) ) ;
#895 = DIRECTION ( 'NONE',  ( 0.000000000000000000, 1.000000000000000000, 0.000000000000000000 ) ) ;
#896 = ORIENTED_EDGE ( 'NONE', *, *, #7076, .T. ) ;
#897 = CARTESIAN_POINT ( 'NONE',  ( 3.500000000000000000, -6.950659073900639306, -0.01814118441313969030 ) ) ;
#898 = CARTESIAN_POINT ( 'NONE',  ( 1.406733260263402174, -27.08258545099816672, 5.249999999999995559 ) ) ;
#899 = AXIS2_PLACEMENT_3D ( 'NONE', #5052, #7905, #6359 ) ;
#900 = CARTESIAN_POINT ( 'NONE',  ( -5.114683531250000748, -28.23437500034139447, -6.263680815196995234E-16 ) ) ;
#901 = EDGE_CURVE ( 'NONE', #6843, #5960, #176, .T. ) ;
#902 = ORIENTED_EDGE ( 'NONE', *, *, #6341, .F. ) ;
#903 = DIRECTION ( 'NONE',  ( 1.000000000000000000, 0.000000000000000000, 0.000000000000000000 ) ) ;
#904 = CARTESIAN_POINT ( 'NONE',  ( -5.385316468750000141, -27.85937499965860198, 0.000000000000000000 ) ) ;
#905 = EDGE_CURVE ( 'NONE', #8760, #6742, #5895, .T. ) ;
#906 = CARTESIAN_POINT ( 'NONE',  ( -4.000000000000000000, -4.550659073900638951, 0.01814118441313491634 ) ) ;
#907 = CARTESIAN_POINT ( 'NONE',  ( 2.625000000000000444, -27.45833333333333215, -4.546633369868303021 ) ) ;
#908 = ORIENTED_EDGE ( 'NONE', *, *, #7926, .T. ) ;
#909 = CARTESIAN_POINT ( 'NONE',  ( 0.000000000000000000, 75.00000000000000000, 0.000000000000000000 ) ) ;
#910 = CARTESIAN_POINT ( 'NONE',  ( 0.000000000000000000, 0.000000000000000000, 0.000000000000000000 ) ) ;
#911 = CARTESIAN_POINT ( 'NONE',  ( -5.385316468750001029, -27.38020833299193768, -3.109213912904136734 ) ) ;
#912 = CARTESIAN_POINT ( 'NONE',  ( -5.114683531250000748, -29.79687500034139802, -6.263680815196995234E-16 ) ) ;
#913 = DIRECTION ( 'NONE',  ( 0.000000000000000000, 0.000000000000000000, -1.000000000000000000 ) ) ;
#914 = CARTESIAN_POINT ( 'NONE',  ( -5.385316468749998364, -27.55729166632526628, 3.109213912904140287 ) ) ;
#915 = CARTESIAN_POINT ( 'NONE',  ( 1.224499502706142273, -0.8506590739006396618, -3.007514324621435531 ) ) ;
#916 = CARTESIAN_POINT ( 'NONE',  ( 1.975475456537005874E-15, -27.37499999931720041, 5.250000000000000000 ) ) ;
#917 = CARTESIAN_POINT ( 'NONE',  ( 4.007514324621432422, -6.850659073900641438, 1.638713065079246078 ) ) ;
#918 = CARTESIAN_POINT ( 'NONE',  ( -2.625000000000000444, -27.47916666598386826, -4.546633369868303021 ) ) ;
#919 = CARTESIAN_POINT ( 'NONE',  ( 3.367778697655221012E-16, -28.00000000000000000, 2.750000000000000000 ) ) ;
#920 = CARTESIAN_POINT ( 'NONE',  ( -1.467888652719046449, -3.749340926099361315, 3.492485675378535603 ) ) ;
#921 = CARTESIAN_POINT ( 'NONE',  ( 1.836970198721030181E-16, 70.00000000000000000, 1.500000000000000222 ) ) ;
#922 = ORIENTED_EDGE ( 'NONE', *, *, #8343, .T. ) ;
#923 = CARTESIAN_POINT ( 'NONE',  ( -2.692658234375000514, -28.11979166632526628, -4.663820869356205989 ) ) ;
#924 = EDGE_CURVE ( 'NONE', #8014, #8128, #5623, .T. ) ;
#925 = CARTESIAN_POINT ( 'NONE',  ( 2.841254879263533262, -4.449340926099361937, -2.815599370228847320 ) ) ;
#926 = DIRECTION ( 'NONE',  ( 0.000000000000000000, 1.000000000000000000, 0.000000000000000000 ) ) ;
#927 = ORIENTED_EDGE ( 'NONE', *, *, #5310, .F. ) ;
#928 = CARTESIAN_POINT ( 'NONE',  ( -2.624999999999996891, -27.20833333333333570, 4.546633369868304797 ) ) ;
#929 = CARTESIAN_POINT ( 'NONE',  ( -2.134148098076932953, -5.950659073900640195, -2.108492589042352705 ) ) ;
#930 = AXIS2_PLACEMENT_3D ( 'NONE', #8253, #4020, #5403 ) ;
#931 = ORIENTED_EDGE ( 'NONE', *, *, #6120, .T. ) ;
#932 = CARTESIAN_POINT ( 'NONE',  ( -1.113604000661152470E-15, -27.81250000000000000, 6.062177826491070398 ) ) ;
#933 = EDGE_CURVE ( 'NONE', #2936, #3199, #6596, .T. ) ;
#934 = CARTESIAN_POINT ( 'NONE',  ( -5.114683531250001636, -28.52604166700806587, 2.952963913586931444 ) ) ;
#935 = CIRCLE ( 'NONE', #5240, 0.2499999999999998335 ) ;
#936 = PRESENTATION_LAYER_ASSIGNMENT (  '', '', ( #5984 ) ) ;
#937 = FILL_AREA_STYLE ('',( #5863 ) ) ;
#938 = CARTESIAN_POINT ( 'NONE',  ( 5.250000000000000888, -27.14583333333333570, 3.031088913245532979 ) ) ;
#939 = CARTESIAN_POINT ( 'NONE',  ( 0.000000000000000000, -30.00000000000000000, 0.000000000000000000 ) ) ;
#940 = CARTESIAN_POINT ( 'NONE',  ( -3.500000000000000000, -3.449340926099361049, -0.01814118441321344033 ) ) ;
#941 = CARTESIAN_POINT ( 'NONE',  ( 6.429395695523604153E-16, -27.00000000000000000, 5.250000000000000000 ) ) ;
#942 = CARTESIAN_POINT ( 'NONE',  ( -5.250000000000000000, -28.25000000000000000, 0.000000000000000000 ) ) ;
#943 = CARTESIAN_POINT ( 'NONE',  ( 5.114683531249999859, -28.40104166700806232, -2.952963913586932776 ) ) ;
#944 = DIRECTION ( 'NONE',  ( 0.000000000000000000, 1.000000000000000000, 0.000000000000000000 ) ) ;
#945 = AXIS2_PLACEMENT_3D ( 'NONE', #2361, #8822, #2458 ) ;
#946 = VERTEX_POINT ( 'NONE', #226 ) ;
#947 = CARTESIAN_POINT ( 'NONE',  ( 2.624999999999996891, -27.07291666734946389, 4.546633369868304797 ) ) ;
#948 = CARTESIAN_POINT ( 'NONE',  ( -5.114683531250000748, -28.98437500034139802, -6.263680815196995234E-16 ) ) ;
#949 = ORIENTED_EDGE ( 'NONE', *, *, #4125, .F. ) ;
#950 = DIRECTION ( 'NONE',  ( 0.000000000000000000, -1.000000000000000000, 0.000000000000000000 ) ) ;
#951 = CARTESIAN_POINT ( 'NONE',  ( -5.385316468750001029, -27.38020833299193058, -3.109213912904136734 ) ) ;
#952 = CARTESIAN_POINT ( 'NONE',  ( -1.674995433905516196, -2.650659073900639040, -3.992485675378566690 ) ) ;
#953 = CARTESIAN_POINT ( 'NONE',  ( -1.406733260263387963, -29.17633545031536713, -5.250000000000001776 ) ) ;
#954 = ORIENTED_EDGE ( 'NONE', *, *, #1054, .F. ) ;
#955 = DIRECTION ( 'NONE',  ( 0.000000000000000000, -1.000000000000000000, 0.000000000000000000 ) ) ;
#956 = CARTESIAN_POINT ( 'NONE',  ( -2.625000000000002220, -28.86458333401612819, 4.546633369868302132 ) ) ;
#957 = EDGE_CURVE ( 'NONE', #7496, #1130, #5197, .T. ) ;
#958 = CARTESIAN_POINT ( 'NONE',  ( 5.385316468749999252, -27.71354166632526272, -3.109213912904139399 ) ) ;
#959 = CARTESIAN_POINT ( 'NONE',  ( 5.114683531250000748, -27.35937500034139802, 0.000000000000000000 ) ) ;
#960 = ORIENTED_EDGE ( 'NONE', *, *, #7717, .F. ) ;
#961 = CARTESIAN_POINT ( 'NONE',  ( -2.692658234374996518, -27.53645833299193413, 4.663820869356208654 ) ) ;
#962 = CARTESIAN_POINT ( 'NONE',  ( -3.000000000000000444, -4.550659073900638951, 0.01814118441314532468 ) ) ;
#963 = DIRECTION ( 'NONE',  ( 0.000000000000000000, 1.000000000000000000, 0.000000000000000000 ) ) ;
#964 = CARTESIAN_POINT ( 'NONE',  ( 5.250000000000000000, -27.29166666598386826, -3.031088913245536531 ) ) ;
#965 = CARTESIAN_POINT ( 'NONE',  ( 1.975475456537005874E-15, -27.62499999931720041, 5.250000000000000000 ) ) ;
#966 = CARTESIAN_POINT ( 'NONE',  ( 1.431606283892619347, -2.349340926099361404, 3.507514324621464397 ) ) ;
#967 = CARTESIAN_POINT ( 'NONE',  ( -2.033577675846918216E-14, -29.87499999931720396, 5.250000000000000888 ) ) ;
#968 = ORIENTED_EDGE ( 'NONE', *, *, #8122, .T. ) ;
#969 = SURFACE_STYLE_USAGE ( .BOTH. , #8693 ) ;
#970 = CARTESIAN_POINT ( 'NONE',  ( 2.692658234375002735, -28.24479166632526628, 4.663820869356205101 ) ) ;
#971 = ADVANCED_FACE ( 'NONE', ( #8322 ), #8915, .F. ) ;
#972 = CARTESIAN_POINT ( 'NONE',  ( -2.815599370228846876, -6.449340926099361049, -2.841254879263533262 ) ) ;
#973 = CARTESIAN_POINT ( 'NONE',  ( 4.898587196589411843E-16, 1.000000000000000000, 3.999999999999999112 ) ) ;
#974 = EDGE_LOOP ( 'NONE', ( #8366, #1071 ) ) ;
#975 = CARTESIAN_POINT ( 'NONE',  ( 2.692658234374998738, -28.91145833299193413, -4.663820869356206877 ) ) ;
#976 = CARTESIAN_POINT ( 'NONE',  ( 1.260781871532430598, -5.050659073900640728, 2.992485675378564469 ) ) ;
#977 = VERTEX_POINT ( 'NONE', #4824 ) ;
#978 = CARTESIAN_POINT ( 'NONE',  ( 3.712013335537174572E-16, -28.18749999999999645, -6.062177826491070398 ) ) ;
#979 = CARTESIAN_POINT ( 'NONE',  ( -1.467888652718973841, -1.050659073900639173, -3.492485675378565801 ) ) ;
#980 = CARTESIAN_POINT ( 'NONE',  ( -2.324088772396477476E-15, -29.46875000068279959, -5.250000000000000000 ) ) ;
#981 = CARTESIAN_POINT ( 'NONE',  ( -2.557341765624999042, -28.52604166700806587, -4.429445870380400052 ) ) ;
#982 =( BOUNDED_CURVE ( )  B_SPLINE_CURVE ( 2, ( #6188, #1260, #4831, #7587, #2619, #8921, #5436, #6273, #2006 ),
 .UNSPECIFIED., .F., .F. ) 
 B_SPLINE_CURVE_WITH_KNOTS ( ( 3, 2, 2, 2, 3 ),
 ( 0.3125000000000000000, 0.3194444444444444198, 0.3333333333333333148, 0.3472222222222222099, 0.3541666666666666852 ),
 .UNSPECIFIED. ) 
 CURVE ( )  GEOMETRIC_REPRESENTATION_ITEM ( )  RATIONAL_B_SPLINE_CURVE ( ( 0.9330127018922194093, 0.9330127018922194093, 1.000000000000000000, 0.8660254037844387076, 1.000000000000000000, 0.8660254037844387076, 1.000000000000000000, 0.9330127018922190762, 0.9330127018922194093 ) ) 
 REPRESENTATION_ITEM ( '' )  );
#983 = CARTESIAN_POINT ( 'NONE',  ( -3.492485675378536047, -3.349340926099361404, -1.467888652719048670 ) ) ;
#984 = CARTESIAN_POINT ( 'NONE',  ( 5.249999999999997335, -28.80208333401612819, 3.031088913245538308 ) ) ;
#985 = CARTESIAN_POINT ( 'NONE',  ( -1.406733260263394625, -28.30133545031536713, -5.250000000000000000 ) ) ;
#986 = CARTESIAN_POINT ( 'NONE',  ( -5.114683531250000748, -29.04687500034139802, -6.263680815196995234E-16 ) ) ;
#987 = DIRECTION ( 'NONE',  ( 0.000000000000000000, -1.000000000000000000, 0.000000000000000000 ) ) ;
#988 = ORIENTED_EDGE ( 'NONE', *, *, #517, .T. ) ;
#989 = FACE_BOUND ( 'NONE', #6645, .T. ) ;
#990 = CARTESIAN_POINT ( 'NONE',  ( -5.114683531250000748, -28.46354166700806587, 2.952963913586931888 ) ) ;
#991 =( REPRESENTATION_RELATIONSHIP ('NONE','NONE', #735, #6994 ) REPRESENTATION_RELATIONSHIP_WITH_TRANSFORMATION ( #5747 )SHAPE_REPRESENTATION_RELATIONSHIP( ) );
#992 = ORIENTED_EDGE ( 'NONE', *, *, #8749, .T. ) ;
#993 = CYLINDRICAL_SURFACE ( 'NONE', #5848, 5.250000000000000000 ) ;
#994 = CARTESIAN_POINT ( 'NONE',  ( 2.692658234374998738, -27.69270833299193768, -4.663820869356206877 ) ) ;
#995 = CARTESIAN_POINT ( 'NONE',  ( 4.000000000000000000, -2.150659073900639040, -0.01814118441313441674 ) ) ;
#996 = UNCERTAINTY_MEASURE_WITH_UNIT (LENGTH_MEASURE( 1.000000000000000082E-05 ), #5266, 'distance_accuracy_value', 'NONE');
#997 = CARTESIAN_POINT ( 'NONE',  ( -1.000000000000000000, -29.00000000000000355, -3.048902179152658931 ) ) ;
#998 = CARTESIAN_POINT ( 'NONE',  ( -3.807688866302469071E-16, -27.92187499965860198, -6.218427825808274356 ) ) ;
#999 = ORIENTED_EDGE ( 'NONE', *, *, #4125, .T. ) ;
#1000 = EDGE_CURVE ( 'NONE', #4607, #791, #3032, .T. ) ;
#1001 = CARTESIAN_POINT ( 'NONE',  ( 0.000000000000000000, -30.00000000000000000, 0.000000000000000000 ) ) ;
#1002 = DIRECTION ( 'NONE',  ( 0.000000000000000000, -1.000000000000000000, 0.000000000000000000 ) ) ;
#1003 = CARTESIAN_POINT ( 'NONE',  ( -5.385316468749998364, -28.33854166632526628, 3.109213912904140287 ) ) ;
#1004 = CARTESIAN_POINT ( 'NONE',  ( -5.114683531249999859, -29.06770833367473017, -2.952963913586935440 ) ) ;
#1005 = EDGE_LOOP ( 'NONE', ( #5857, #7682, #7845, #1554 ) ) ;
#1006 = DIRECTION ( 'NONE',  ( 0.000000000000000000, 1.000000000000000000, 0.000000000000000000 ) ) ;
#1007 = CARTESIAN_POINT ( 'NONE',  ( -3.007514324621435531, -1.250659073900639573, -1.224499502706142273 ) ) ;
#1008 = DIRECTION ( 'NONE',  ( 0.000000000000000000, 0.000000000000000000, 1.000000000000000000 ) ) ;
#1009 = PRODUCT_DEFINITION_FORMATION_WITH_SPECIFIED_SOURCE ( 'ANY', '', #1433, .NOT_KNOWN. ) ;
#1010 = CARTESIAN_POINT ( 'NONE',  ( -5.250000000000000000, -27.70833333265053611, -3.031088913245534755 ) ) ;
#1011 = CYLINDRICAL_SURFACE ( 'NONE', #6584, 5.250000000000000000 ) ;
#1012 = DIRECTION ( 'NONE',  ( 0.000000000000000000, 0.000000000000000000, -1.000000000000000000 ) ) ;
#1013 = CARTESIAN_POINT ( 'NONE',  ( 1.406733260263385521, -29.11383544963257464, 5.250000000000006217 ) ) ;
#1014 = CYLINDRICAL_SURFACE ( 'NONE', #6247, 5.750000000000000000 ) ;
#1015 = CARTESIAN_POINT ( 'NONE',  ( 0.000000000000000000, 0.000000000000000000, 0.000000000000000000 ) ) ;
#1016 = CARTESIAN_POINT ( 'NONE',  ( -5.385316468749998364, -28.05729166632526983, 3.109213912904140287 ) ) ;
#1017 = CARTESIAN_POINT ( 'NONE',  ( -2.815599370228846876, -1.649340926099360560, -2.841254879263533262 ) ) ;
#1018 = CARTESIAN_POINT ( 'NONE',  ( -9.180150650966086169E-15, -28.43750000000000000, 5.250000000000000000 ) ) ;
#1019 = ORIENTED_EDGE ( 'NONE', *, *, #3908, .F. ) ;
#1020 = CARTESIAN_POINT ( 'NONE',  ( -5.385316468750000141, -27.82812499965860198, 0.000000000000000000 ) ) ;
#1021 = CARTESIAN_POINT ( 'NONE',  ( 0.01814118441313990887, -4.950659073900639306, 3.500000000000000000 ) ) ;
#1022 = ORIENTED_EDGE ( 'NONE', *, *, #4471, .T. ) ;
#1023 = CARTESIAN_POINT ( 'NONE',  ( 2.624999999999996891, -28.04166666666666785, 4.546633369868304797 ) ) ;
#1024 = AXIS2_PLACEMENT_3D ( 'NONE', #6724, #963, #8824 ) ;
#1025 = CARTESIAN_POINT ( 'NONE',  ( 0.01814118441313990887, -0.1506590739006389568, 3.500000000000000000 ) ) ;
#1026 = ORIENTED_EDGE ( 'NONE', *, *, #3740, .T. ) ;
#1027 = COLOUR_RGB ( '',0.8941176470588234615, 0.8941176470588234615, 0.8941176470588234615 ) ;
#1028 = CARTESIAN_POINT ( 'NONE',  ( 5.250000000000000888, -27.39583333333333215, 3.031088913245532979 ) ) ;
#1029 = EDGE_LOOP ( 'NONE', ( #277, #4373, #5520, #6752, #7836, #4879, #5582, #4542 ) ) ;
#1030 = CARTESIAN_POINT ( 'NONE',  ( 5.114683531249998971, -28.38020833367473017, 2.952963913586936329 ) ) ;
#1031 = CARTESIAN_POINT ( 'NONE',  ( -3.500000000000000000, -5.049340926099361582, -0.01814118441321344033 ) ) ;
#1032 = DIRECTION ( 'NONE',  ( 0.000000000000000000, 0.000000000000000000, 1.000000000000000000 ) ) ;
#1033 = CARTESIAN_POINT ( 'NONE',  ( -1.975475456537005874E-15, -27.56249999999999289, 5.249999999999999112 ) ) ;
#1034 = CARTESIAN_POINT ( 'NONE',  ( -2.557341765625002594, -28.50520833367473017, 4.429445870380399164 ) ) ;
#1035 = ORIENTED_EDGE ( 'NONE', *, *, #6208, .T. ) ;
#1036 = DIRECTION ( 'NONE',  ( 0.000000000000000000, 0.000000000000000000, -1.000000000000000000 ) ) ;
#1037 = CARTESIAN_POINT ( 'NONE',  ( 5.114683531249998971, -27.63020833367473017, 2.952963913586936329 ) ) ;
#1038 = VECTOR ( 'NONE', #2949, 1000.000000000000000 ) ;
#1039 =( BOUNDED_CURVE ( )  B_SPLINE_CURVE ( 2, ( #3080, #1723, #3126, #5902, #2469, #8789, #8741, #5856, #8144 ),
 .UNSPECIFIED., .F., .F. ) 
 B_SPLINE_CURVE_WITH_KNOTS ( ( 3, 2, 2, 2, 3 ),
 ( 0.8541666666666666297, 0.8611111111111111605, 0.8750000000000000000, 0.8888888888888888395, 0.8958333333333333703 ),
 .UNSPECIFIED. ) 
 CURVE ( )  GEOMETRIC_REPRESENTATION_ITEM ( )  RATIONAL_B_SPLINE_CURVE ( ( 0.9330127018922192983, 0.9330127018922187432, 1.000000000000000000, 0.8660254037844387076, 1.000000000000000000, 0.8660254037844387076, 1.000000000000000000, 0.9330127018922187432, 0.9330127018922192983 ) ) 
 REPRESENTATION_ITEM ( '' )  );
#1040 = ORIENTED_EDGE ( 'NONE', *, *, #7385, .T. ) ;
#1041 = CYLINDRICAL_SURFACE ( 'NONE', #7416, 3.000000000000000444 ) ;
#1042 = CLOSED_SHELL ( 'NONE', ( #5130, #1686, #496, #8751, #6627 ) ) ;
#1043 = ADVANCED_FACE ( 'NONE', ( #1954 ), #6130, .T. ) ;
#1044 = CARTESIAN_POINT ( 'NONE',  ( -5.385316468749998364, -28.33854166632526628, 3.109213912904140287 ) ) ;
#1045 = CARTESIAN_POINT ( 'NONE',  ( 4.000000000000000000, -1.049340926099360916, 0.01814118441321914063 ) ) ;
#1046 = DIRECTION ( 'NONE',  ( 0.000000000000000000, 1.000000000000000000, 0.000000000000000000 ) ) ;
#1047 = CARTESIAN_POINT ( 'NONE',  ( -5.385316468749998364, -28.33854166632526628, 3.109213912904140287 ) ) ;
#1048 = ORIENTED_EDGE ( 'NONE', *, *, #8424, .T. ) ;
#1049 = VECTOR ( 'NONE', #483, 1000.000000000000000 ) ;
#1050 = EDGE_CURVE ( 'NONE', #7374, #3248, #5428, .T. ) ;
#1051 = CARTESIAN_POINT ( 'NONE',  ( 1.406733260263391960, -29.33258545099816317, 5.250000000000000000 ) ) ;
#1052 = CARTESIAN_POINT ( 'NONE',  ( 5.250000000000000000, -28.01041666734946389, -3.031088913245534755 ) ) ;
#1053 = CARTESIAN_POINT ( 'NONE',  ( -2.692658234375000514, -27.90104166632526628, -4.663820869356205989 ) ) ;
#1054 = EDGE_CURVE ( 'NONE', #2054, #7800, #8781, .T. ) ;
#1055 = UNCERTAINTY_MEASURE_WITH_UNIT (LENGTH_MEASURE( 1.000000000000000082E-05 ), #5104, 'distance_accuracy_value', 'NONE');
#1056 = VERTEX_POINT ( 'NONE', #3998 ) ;
#1057 = AXIS2_PLACEMENT_3D ( 'NONE', #2801, #6450, #3581 ) ;
#1058 = CARTESIAN_POINT ( 'NONE',  ( -5.385316468750000141, -27.82812499965860198, 0.000000000000000000 ) ) ;
#1059 = CARTESIAN_POINT ( 'NONE',  ( 2.108492589042352705, -2.350659073900639218, -2.134148098076933397 ) ) ;
#1060 = CYLINDRICAL_SURFACE ( 'NONE', #433, 2.750000000000000000 ) ;
#1061 = CARTESIAN_POINT ( 'NONE',  ( 2.624999999999998668, -27.52083333265053611, -4.546633369868303021 ) ) ;
#1062 = CARTESIAN_POINT ( 'NONE',  ( 5.114683531250000748, -29.92187500034139802, 0.000000000000000000 ) ) ;
#1063 = CARTESIAN_POINT ( 'NONE',  ( 1.431606283892619347, -5.549340926099361582, 3.507514324621464397 ) ) ;
#1064 = CARTESIAN_POINT ( 'NONE',  ( 3.616337804771879580E-16, -29.54687500034139802, -5.905927827173866440 ) ) ;
#1065 = ORIENTED_EDGE ( 'NONE', *, *, #1265, .F. ) ;
#1066 =( NAMED_UNIT ( * ) SI_UNIT ( $, .STERADIAN. ) SOLID_ANGLE_UNIT ( ) );
#1067 =( BOUNDED_CURVE ( )  B_SPLINE_CURVE ( 2, ( #2665, #1920, #5537, #4010, #2757, #7722, #6844, #3964, #1877, #5392, #1965 ),
 .UNSPECIFIED., .F., .F. ) 
 B_SPLINE_CURVE_WITH_KNOTS ( ( 3, 2, 2, 2, 2, 3 ),
 ( 0.9375000002123526910, 0.9444444444444444198, 0.9583333333333333703, 0.9722222222222222099, 0.9861111111111111605, 1.000000000000000000 ),
 .UNSPECIFIED. ) 
 CURVE ( )  GEOMETRIC_REPRESENTATION_ITEM ( )  RATIONAL_B_SPLINE_CURVE ( ( 0.9330127018922194093, 0.9330127039406097555, 1.000000000000000000, 0.8660254037844387076, 1.000000000000000000, 0.8660254037844387076, 1.000000000000000000, 0.8660254037844387076, 1.000000000000000000, 0.8660254037844387076, 1.000000000000000000 ) ) 
 REPRESENTATION_ITEM ( '' )  );
#1068 = CARTESIAN_POINT ( 'NONE',  ( -2.692658234375000514, -28.36979166632526628, -4.663820869356205989 ) ) ;
#1069 = CARTESIAN_POINT ( 'NONE',  ( -0.01814118441321889430, -2.249340926099360427, 4.000000000000000000 ) ) ;
#1070 = CARTESIAN_POINT ( 'NONE',  ( 0.000000000000000000, -47.00000000000000000, 2.549999999999999822 ) ) ;
#1071 = ORIENTED_EDGE ( 'NONE', *, *, #1671, .T. ) ;
#1072 = CARTESIAN_POINT ( 'NONE',  ( -3.807688866302469071E-16, -27.89062499965860198, -6.218427825808274356 ) ) ;
#1073 = CARTESIAN_POINT ( 'NONE',  ( -2.462045979635629323, -4.750659073900639129, 2.487701488670203798 ) ) ;
#1074 = VERTEX_POINT ( 'NONE', #457 ) ;
#1075 = CARTESIAN_POINT ( 'NONE',  ( -5.250000000000000888, -27.35416666666666430, 3.031088913245532979 ) ) ;
#1076 = CARTESIAN_POINT ( 'NONE',  ( -5.250000000000000888, -28.63541666734946389, 3.031088913245533423 ) ) ;
#1077 = EDGE_CURVE ( 'NONE', #791, #6502, #552, .T. ) ;
#1078 = CARTESIAN_POINT ( 'NONE',  ( -1.084901341431563726E-15, -26.98437500034139802, 5.905927827173866440 ) ) ;
#1079 = ORIENTED_EDGE ( 'NONE', *, *, #8052, .F. ) ;
#1080 =( LENGTH_UNIT ( ) NAMED_UNIT ( * ) SI_UNIT ( .MILLI., .METRE. ) );
#1081 = CARTESIAN_POINT ( 'NONE',  ( -3.712013335537174572E-16, -27.06250000000000000, -6.062177826491070398 ) ) ;
#1082 = EDGE_LOOP ( 'NONE', ( #8172, #4837 ) ) ;
#1083 = CARTESIAN_POINT ( 'NONE',  ( 2.557341765625000818, -28.81770833367473017, -4.429445870380400052 ) ) ;
#1084 = CARTESIAN_POINT ( 'NONE',  ( -2.992485675378538268, -4.949340926099361937, -1.260781871532495879 ) ) ;
#1085 = DIRECTION ( 'NONE',  ( 0.000000000000000000, -1.000000000000000000, 0.000000000000000000 ) ) ;
#1086 = DIRECTION ( 'NONE',  ( 0.000000000000000000, 0.000000000000000000, -1.000000000000000000 ) ) ;
#1087 = CARTESIAN_POINT ( 'NONE',  ( -2.557341765624999042, -29.08854166700806587, -4.429445870380400052 ) ) ;
#1088 = FACE_OUTER_BOUND ( 'NONE', #5599, .T. ) ;
#1089 = AXIS2_PLACEMENT_3D ( 'NONE', #939, #8612, #148 ) ;
#1090 = CARTESIAN_POINT ( 'NONE',  ( -2.075653704136731559, -4.858300672349190065E-16, 2.699248787648522274 ) ) ;
#1091 = CARTESIAN_POINT ( 'NONE',  ( -2.557341765624999042, -27.27604166700806587, -4.429445870380400052 ) ) ;
#1092 = ORIENTED_EDGE ( 'NONE', *, *, #3526, .F. ) ;
#1093 = AXIS2_PLACEMENT_3D ( 'NONE', #2218, #8727, #913 ) ;
#1094 = DIRECTION ( 'NONE',  ( 0.000000000000000000, 1.000000000000000000, 0.000000000000000000 ) ) ;
#1095 = CARTESIAN_POINT ( 'NONE',  ( -3.807688866302469071E-16, -29.17187499965859843, -6.218427825808274356 ) ) ;
#1096 = CARTESIAN_POINT ( 'NONE',  ( 5.385316468750000141, -29.73437499965859843, -6.595110575850215044E-16 ) ) ;
#1097=STYLED_ITEM('',(#9239),#5214);
#1098 = DIRECTION ( 'NONE',  ( 0.000000000000000000, 0.000000000000000000, -1.000000000000000000 ) ) ;
#1099 = CARTESIAN_POINT ( 'NONE',  ( 5.385316468750001029, -29.50520833299193413, 3.109213912904135846 ) ) ;
#1100 = CARTESIAN_POINT ( 'NONE',  ( -0.01814118441321889430, -3.849340926099360960, 4.000000000000000000 ) ) ;
#1101 = ORIENTED_EDGE ( 'NONE', *, *, #2223, .F. ) ;
#1102 = DIRECTION ( 'NONE',  ( 0.000000000000000000, -1.000000000000000000, 0.000000000000000000 ) ) ;
#1103 = CARTESIAN_POINT ( 'NONE',  ( -2.624999999999998668, -27.44791666734946389, -4.546633369868303021 ) ) ;
#1104 = CARTESIAN_POINT ( 'NONE',  ( -2.692658234374996518, -28.81770833299193413, 4.663820869356208654 ) ) ;
#1105 = VECTOR ( 'NONE', #4491, 1000.000000000000000 ) ;
#1106 = ORIENTED_EDGE ( 'NONE', *, *, #6600, .F. ) ;
#1107 = CARTESIAN_POINT ( 'NONE',  ( -3.807688866302469071E-16, -28.14062499965860198, -6.218427825808274356 ) ) ;
#1108 = CARTESIAN_POINT ( 'NONE',  ( 1.431606283892694842, -2.450659073900638862, -3.507514324621434199 ) ) ;
#1109 = CARTESIAN_POINT ( 'NONE',  ( -1.975475456537005874E-15, -29.06249999999999645, 5.249999999999999112 ) ) ;
#1110 = ADVANCED_FACE ( 'NONE', ( #1205 ), #4091, .F. ) ;
#1111 = SURFACE_STYLE_FILL_AREA ( #2505 ) ;
#1112 = DIRECTION ( 'NONE',  ( 0.000000000000000000, 1.000000000000000000, 0.000000000000000000 ) ) ;
#1113 = CARTESIAN_POINT ( 'NONE',  ( 3.507514324621465285, -7.549340926099361582, -1.431606283892619347 ) ) ;
#1114 = CARTESIAN_POINT ( 'NONE',  ( -5.114683531250000748, -29.46354166700806232, 2.952963913586931888 ) ) ;
#1115 = CYLINDRICAL_SURFACE ( 'NONE', #2552, 3.999999999999999112 ) ;
#1116 = CARTESIAN_POINT ( 'NONE',  ( 5.385316468750000141, -29.95312499965859843, -6.595110575850215044E-16 ) ) ;
#1117 = CARTESIAN_POINT ( 'NONE',  ( -0.01814118441321365544, -3.849340926099361404, 3.500000000000000000 ) ) ;
#1118 = CARTESIAN_POINT ( 'NONE',  ( -5.249999999999997335, -29.47916666666666785, 3.031088913245538308 ) ) ;
#1119 = CARTESIAN_POINT ( 'NONE',  ( 2.692658234375002735, -28.49479166632526628, 4.663820869356205101 ) ) ;
#1120 = EDGE_CURVE ( 'NONE', #2527, #2627, #6233, .T. ) ;
#1121 = CARTESIAN_POINT ( 'NONE',  ( -1.431606283892693066, -6.450659073900639306, 3.507514324621434199 ) ) ;
#1122 = EDGE_LOOP ( 'NONE', ( #3146, #1512, #5729, #3838 ) ) ;
#1123 = CARTESIAN_POINT ( 'NONE',  ( 2.624999999999996891, -27.79166666666666430, 4.546633369868304797 ) ) ;
#1124 = CARTESIAN_POINT ( 'NONE',  ( 0.000000000000000000, -50.00000000000000000, 0.000000000000000000 ) ) ;
#1125 = EDGE_CURVE ( 'NONE', #8145, #1171, #1682, .T. ) ;
#1126 = CARTESIAN_POINT ( 'NONE',  ( 2.462045979635629767, -3.950659073900639751, -2.487701488670203354 ) ) ;
#1127 =( BOUNDED_CURVE ( )  B_SPLINE_CURVE ( 2, ( #482, #6057, #431, #8207, #385, #4579, #7725, #8893, #2536 ),
 .UNSPECIFIED., .F., .T. ) 
 B_SPLINE_CURVE_WITH_KNOTS ( ( 3, 2, 2, 2, 3 ),
 ( 0.6041666666666666297, 0.6111111111111111605, 0.6250000000000000000, 0.6388888888888888395, 0.6458333333333333703 ),
 .UNSPECIFIED. ) 
 CURVE ( )  GEOMETRIC_REPRESENTATION_ITEM ( )  RATIONAL_B_SPLINE_CURVE ( ( 0.9330127018922192983, 0.9330127018922187432, 1.000000000000000000, 0.8660254037844387076, 1.000000000000000000, 0.8660254037844387076, 1.000000000000000000, 0.9330127018922187432, 0.9330127018922192983 ) ) 
 REPRESENTATION_ITEM ( '' )  );
#1128 = ORIENTED_EDGE ( 'NONE', *, *, #1174, .F. ) ;
#1129 = CARTESIAN_POINT ( 'NONE',  ( -5.249999999999999112, -27.97916666666666430, 3.031088913245538308 ) ) ;
#1130 = VERTEX_POINT ( 'NONE', #4733 ) ;
#1131 = CARTESIAN_POINT ( 'NONE',  ( 5.114683531249998971, -28.63020833367473017, 2.952963913586936329 ) ) ;
#1132 = CARTESIAN_POINT ( 'NONE',  ( 2.487701488670255756, -7.649340926099361226, -2.462045979635577364 ) ) ;
#1133 = CARTESIAN_POINT ( 'NONE',  ( 1.406733260263397289, -28.58258545099816672, 5.249999999999997335 ) ) ;
#1134 = CARTESIAN_POINT ( 'NONE',  ( 0.000000000000000000, -47.00000000000000000, 0.000000000000000000 ) ) ;
#1135 = CARTESIAN_POINT ( 'NONE',  ( 2.557341765624996821, -28.46354166700806587, 4.429445870380401828 ) ) ;
#1136 = SURFACE_SIDE_STYLE ('',( #384 ) ) ;
#1137 = CARTESIAN_POINT ( 'NONE',  ( 0.000000000000000000, -35.00000000000000000, 0.000000000000000000 ) ) ;
#1138 = CARTESIAN_POINT ( 'NONE',  ( 2.557341765625000818, -27.31770833367473017, -4.429445870380400052 ) ) ;
#1139 = ORIENTED_EDGE ( 'NONE', *, *, #8338, .T. ) ;
#1140 = CARTESIAN_POINT ( 'NONE',  ( 0.000000000000000000, -47.00000000000000000, -2.999999999999999556 ) ) ;
#1141 = CARTESIAN_POINT ( 'NONE',  ( -5.385316468750000141, -29.35937499965859843, 0.000000000000000000 ) ) ;
#1142 = CARTESIAN_POINT ( 'NONE',  ( -1.406733260263390628, -28.57366454968462577, 5.250000000000001776 ) ) ;
#1143 = LINE ( 'NONE', #6765, #5493 ) ;
#1144 = CARTESIAN_POINT ( 'NONE',  ( -5.385316468750000141, -29.10937499965859843, 0.000000000000000000 ) ) ;
#1145 = CARTESIAN_POINT ( 'NONE',  ( 0.01814118441321938349, -7.849340926099360516, -4.000000000000000000 ) ) ;
#1146 = EDGE_LOOP ( 'NONE', ( #5954, #445, #7952 ) ) ;
#1147 = CARTESIAN_POINT ( 'NONE',  ( -5.250000000000000000, -27.50000000000000000, 0.000000000000000000 ) ) ;
#1148 = CARTESIAN_POINT ( 'NONE',  ( -1.113604000661152470E-15, -28.09375000068279249, 6.062177826491070398 ) ) ;
#1149 = CARTESIAN_POINT ( 'NONE',  ( 2.692658234375002735, -29.02604166632526983, 4.663820869356205101 ) ) ;
#1150 = ORIENTED_EDGE ( 'NONE', *, *, #2707, .F. ) ;
#1151 = CARTESIAN_POINT ( 'NONE',  ( 1.142306659890740623E-15, -28.26562499965860553, 6.218427825808274356 ) ) ;
#1152 = CARTESIAN_POINT ( 'NONE',  ( 2.108492589042352705, -7.150659073900638596, -2.134148098076933397 ) ) ;
#1153 = DIRECTION ( 'NONE',  ( 0.000000000000000000, 0.000000000000000000, 1.000000000000000000 ) ) ;
#1154 = CARTESIAN_POINT ( 'NONE',  ( 2.300847884672513123E-14, -28.18750000000000000, -5.250000000000000000 ) ) ;
#1155 = CARTESIAN_POINT ( 'NONE',  ( 1.406733260263395735, -27.42633545031537068, 5.250000000000000000 ) ) ;
#1156 = CARTESIAN_POINT ( 'NONE',  ( 1.406733260263393070, -29.69866454968462577, -5.250000000000000888 ) ) ;
#1157 = ORIENTED_EDGE ( 'NONE', *, *, #4558, .T. ) ;
#1158 = APPLICATION_PROTOCOL_DEFINITION ( 'draft international standard', 'automotive_design', 1998, #2904 ) ;
#1159 = PRESENTATION_LAYER_ASSIGNMENT (  '', '', ( #7692 ) ) ;
#1160 = CARTESIAN_POINT ( 'NONE',  ( -3.807688866302469071E-16, -29.14062499965860553, -6.218427825808274356 ) ) ;
#1161 = CARTESIAN_POINT ( 'NONE',  ( 3.000000000000000444, -1.049340926099361582, 0.01814118441320859698 ) ) ;
#1162 = DIRECTION ( 'NONE',  ( 0.000000000000000000, -1.000000000000000000, 0.000000000000000000 ) ) ;
#1163 = CARTESIAN_POINT ( 'NONE',  ( 2.692658234374998738, -28.16145833299193413, -4.663820869356206877 ) ) ;
#1164 = CARTESIAN_POINT ( 'NONE',  ( -2.487701488670202910, -5.950659073900639306, -2.462045979635629767 ) ) ;
#1165 = EDGE_CURVE ( 'NONE', #1550, #8808, #7578, .T. ) ;
#1166 = VERTEX_POINT ( 'NONE', #3351 ) ;
#1167 = CARTESIAN_POINT ( 'NONE',  ( -4.916521616868715807E-16, -50.00000000000000000, 2.786798956483056422 ) ) ;
#1168 = DIRECTION ( 'NONE',  ( 0.000000000000000000, 0.000000000000000000, 1.000000000000000000 ) ) ;
#1169 = ADVANCED_FACE ( 'NONE', ( #6181 ), #9008, .F. ) ;
#1170 = CARTESIAN_POINT ( 'NONE',  ( -2.487701488670202910, -1.150659073900638818, -2.462045979635629767 ) ) ;
#1171 = VERTEX_POINT ( 'NONE', #9055 ) ;
#1172 = CARTESIAN_POINT ( 'NONE',  ( 5.250000000000000000, -29.10416666666666785, -3.031088913245536531 ) ) ;
#1173 = ORIENTED_EDGE ( 'NONE', *, *, #1265, .T. ) ;
#1174 = EDGE_CURVE ( 'NONE', #3963, #8455, #1812, .T. ) ;
#1175 = CARTESIAN_POINT ( 'NONE',  ( 3.616337804771879580E-16, -29.29687500034139802, -5.905927827173866440 ) ) ;
#1176 = CARTESIAN_POINT ( 'NONE',  ( 1.260781871532495657, -2.949340926099361937, -2.992485675378538268 ) ) ;
#1177 = CARTESIAN_POINT ( 'NONE',  ( 0.000000000000000000, -30.00000000000000000, 0.000000000000000000 ) ) ;
#1178 = CARTESIAN_POINT ( 'NONE',  ( -2.557341765625002594, -27.00520833367473017, 4.429445870380399164 ) ) ;
#1179 =( BOUNDED_CURVE ( )  B_SPLINE_CURVE ( 2, ( #782, #5710, #8553, #2979, #7859, #5002, #1480, #4324, #7203 ),
 .UNSPECIFIED., .F., .F. ) 
 B_SPLINE_CURVE_WITH_KNOTS ( ( 3, 2, 2, 2, 3 ),
 ( 0.6875000000000000000, 0.6944444444444444198, 0.7083333333333333703, 0.7222222222222222099, 0.7291666666666667407 ),
 .UNSPECIFIED. ) 
 CURVE ( )  GEOMETRIC_REPRESENTATION_ITEM ( )  RATIONAL_B_SPLINE_CURVE ( ( 0.9330127018922194093, 0.9330127018922194093, 1.000000000000000000, 0.8660254037844387076, 1.000000000000000000, 0.8660254037844387076, 1.000000000000000000, 0.9330127018922187432, 0.9330127018922192983 ) ) 
 REPRESENTATION_ITEM ( '' )  );
#1180 = CARTESIAN_POINT ( 'NONE',  ( -2.261299776309945386, -1.321938709600328683E-17, 2.495489592912619070 ) ) ;
#1181 = CARTESIAN_POINT ( 'NONE',  ( -1.084901341431563923E-15, -27.17187500034140157, 5.905927827173866440 ) ) ;
#1182 = CIRCLE ( 'NONE', #724, 3.000000000000000444 ) ;
#1183 = CARTESIAN_POINT ( 'NONE',  ( 5.114683531250000748, -28.67187500034139802, 0.000000000000000000 ) ) ;
#1184 = EDGE_CURVE ( 'NONE', #3304, #2164, #5654, .T. ) ;
#1185 = DIRECTION ( 'NONE',  ( 0.000000000000000000, -0.000000000000000000, -1.000000000000000000 ) ) ;
#1186 = CARTESIAN_POINT ( 'NONE',  ( -3.807688866302469071E-16, -28.67187499965860198, -6.218427825808274356 ) ) ;
#1187 = FACE_BOUND ( 'NONE', #3193, .T. ) ;
#1188 = FACE_OUTER_BOUND ( 'NONE', #7727, .T. ) ;
#1189 = CARTESIAN_POINT ( 'NONE',  ( 1.142306659890740623E-15, -28.79687499965860198, 6.218427825808274356 ) ) ;
#1190 = CARTESIAN_POINT ( 'NONE',  ( -3.500000000000000000, -3.449340926099361049, -0.01814118441321344033 ) ) ;
#1191 = CIRCLE ( 'NONE', #292, 2.500000000000000000 ) ;
#1192 = CARTESIAN_POINT ( 'NONE',  ( -2.462045979635576920, -1.649340926099361004, -2.487701488670255756 ) ) ;
#1193 = ORIENTED_EDGE ( 'NONE', *, *, #1508, .F. ) ;
#1194 = AXIS2_PLACEMENT_3D ( 'NONE', #7137, #7046, #3559 ) ;
#1195 = CARTESIAN_POINT ( 'NONE',  ( 2.624999999999996891, -29.32291666734946034, 4.546633369868304797 ) ) ;
#1196 = CARTESIAN_POINT ( 'NONE',  ( -5.250000000000000000, -28.65625000068279604, -6.429395695523604153E-16 ) ) ;
#1197 = EDGE_CURVE ( 'NONE', #4744, #451, #2789, .T. ) ;
#1198 = CARTESIAN_POINT ( 'NONE',  ( 5.385316468750000141, -29.73437499965859843, -6.595110575850215044E-16 ) ) ;
#1199 = ADVANCED_FACE ( 'NONE', ( #5698 ), #73, .F. ) ;
#1200 = VERTEX_POINT ( 'NONE', #7011 ) ;
#1201 = CARTESIAN_POINT ( 'NONE',  ( 5.385316468750001029, -28.47395833299193413, 3.109213912904134958 ) ) ;
#1202 = CARTESIAN_POINT ( 'NONE',  ( -2.487701488670202910, -1.150659073900638818, -2.462045979635629767 ) ) ;
#1203 = CARTESIAN_POINT ( 'NONE',  ( 0.000000000000000000, -27.00000000000000000, -5.250000000000000000 ) ) ;
#1204 = CARTESIAN_POINT ( 'NONE',  ( -6.972266317189433020E-16, -29.24999999931720396, -5.249999999999999112 ) ) ;
#1205 = FACE_OUTER_BOUND ( 'NONE', #2938, .T. ) ;
#1206 = CARTESIAN_POINT ( 'NONE',  ( 5.250000000000000888, -27.39583333333333570, 3.031088913245533423 ) ) ;
#1207 = AXIS2_PLACEMENT_3D ( 'NONE', #827, #8513, #128 ) ;
#1208 = DIRECTION ( 'NONE',  ( 0.000000000000000000, -0.000000000000000000, -1.000000000000000000 ) ) ;
#1209 = LINE ( 'NONE', #4049, #340 ) ;
#1210 = SHAPE_DEFINITION_REPRESENTATION ( #28, #2490 ) ;
#1211 = CARTESIAN_POINT ( 'NONE',  ( 5.182341765625000818, -29.82031250051209881, 0.000000000000000000 ) ) ;
#1212 = CARTESIAN_POINT ( 'NONE',  ( -3.492485675378536047, -4.949340926099361049, -1.467888652719048670 ) ) ;
#1213 = CARTESIAN_POINT ( 'NONE',  ( -5.250000000000000000, -29.50000000000000000, 0.000000000000000000 ) ) ;
#1214 = CARTESIAN_POINT ( 'NONE',  ( 2.692658234375002735, -29.49479166632526983, 4.663820869356205101 ) ) ;
#1215 = CARTESIAN_POINT ( 'NONE',  ( 1.467888652718972731, -5.050659073900638063, 3.492485675378566246 ) ) ;
#1216 = ORIENTED_EDGE ( 'NONE', *, *, #4101, .T. ) ;
#1217 = CARTESIAN_POINT ( 'NONE',  ( 2.624999999999996891, -27.04166666666666430, 4.546633369868304797 ) ) ;
#1218 = FACE_OUTER_BOUND ( 'NONE', #1222, .T. ) ;
#1219 = CARTESIAN_POINT ( 'NONE',  ( 0.01814118441313990887, -4.950659073900639306, 3.500000000000000000 ) ) ;
#1220 = ORIENTED_EDGE ( 'NONE', *, *, #6666, .T. ) ;
#1221 = CARTESIAN_POINT ( 'NONE',  ( 5.250000000000000888, -28.89583333333333215, 3.031088913245532979 ) ) ;
#1222 = EDGE_LOOP ( 'NONE', ( #5319, #5073, #7446, #1505 ) ) ;
#1223 = CARTESIAN_POINT ( 'NONE',  ( 2.557341765624996821, -28.15104166700806587, 4.429445870380401828 ) ) ;
#1224 = CARTESIAN_POINT ( 'NONE',  ( 2.992485675378538712, -4.149340926099362115, 1.260781871532494103 ) ) ;
#1225 = CARTESIAN_POINT ( 'NONE',  ( 0.000000000000000000, -30.00000000000000000, 0.000000000000000000 ) ) ;
#1226 = CARTESIAN_POINT ( 'NONE',  ( -2.557341765624999042, -27.58854166700806587, -4.429445870380400052 ) ) ;
#1227 = DIRECTION ( 'NONE',  ( 0.000000000000000000, 0.000000000000000000, 1.000000000000000000 ) ) ;
#1228 = EDGE_CURVE ( 'NONE', #3224, #5282, #7468, .T. ) ;
#1229 = CARTESIAN_POINT ( 'NONE',  ( -5.114683531250000748, -27.71354166700806587, 2.952963913586931888 ) ) ;
#1230 = DIRECTION ( 'NONE',  ( 0.000000000000000000, 0.000000000000000000, 1.000000000000000000 ) ) ;
#1231 = CARTESIAN_POINT ( 'NONE',  ( 2.557341765625000818, -29.38020833367473017, -4.429445870380400052 ) ) ;
#1232 = CARTESIAN_POINT ( 'NONE',  ( 0.000000000000000000, 69.99999999999998579, 0.000000000000000000 ) ) ;
#1233 = CARTESIAN_POINT ( 'NONE',  ( 1.142306659890740623E-15, -29.04687499965859843, 6.218427825808274356 ) ) ;
#1234 = CARTESIAN_POINT ( 'NONE',  ( 1.142306659890740623E-15, -29.79687499965859843, 6.218427825808274356 ) ) ;
#1235 = LINE ( 'NONE', #3240, #2069 ) ;
#1236 = CARTESIAN_POINT ( 'NONE',  ( -5.385316468750000141, -29.35937499965859843, 0.000000000000000000 ) ) ;
#1237 = CARTESIAN_POINT ( 'NONE',  ( 1.431606283892619125, -5.549340926099361582, 3.507514324621464397 ) ) ;
#1238 = CARTESIAN_POINT ( 'NONE',  ( -1.431606283892620235, -1.549340926099361138, -3.507514324621463953 ) ) ;
#1239 = AXIS2_PLACEMENT_3D ( 'NONE', #1225, #6705, #6155 ) ;
#1240 = ORIENTED_EDGE ( 'NONE', *, *, #8391, .F. ) ;
#1241 = DIRECTION ( 'NONE',  ( 0.000000000000000000, 0.000000000000000000, -1.000000000000000000 ) ) ;
#1242 = CARTESIAN_POINT ( 'NONE',  ( 5.250000000000000000, -28.51041666734946389, -3.031088913245534755 ) ) ;
#1243 = CARTESIAN_POINT ( 'NONE',  ( 5.385316468750001029, -28.75520833299193413, 3.109213912904135846 ) ) ;
#1244 = CIRCLE ( 'NONE', #500, 2.750000000000000000 ) ;
#1245 = VECTOR ( 'NONE', #7791, 1000.000000000000000 ) ;
#1246 = ORIENTED_EDGE ( 'NONE', *, *, #6279, .T. ) ;
#1247 = CARTESIAN_POINT ( 'NONE',  ( 5.385316468749999252, -27.93229166632526628, -3.109213912904138954 ) ) ;
#1248 = CARTESIAN_POINT ( 'NONE',  ( -3.500000000000000000, 0.2493409260993610654, 0.01814118441314012051 ) ) ;
#1249 = EDGE_CURVE ( 'NONE', #1724, #4568, #3611, .T. ) ;
#1250 = CARTESIAN_POINT ( 'NONE',  ( 5.249999999999999112, -29.47916666666666430, -3.031088913245534755 ) ) ;
#1251 = AXIS2_PLACEMENT_3D ( 'NONE', #3620, #641, #4139 ) ;
#1252 = PRESENTATION_STYLE_ASSIGNMENT (( #4131 ) ) ;
#1253 = CARTESIAN_POINT ( 'NONE',  ( 0.000000000000000000, -46.00000000000000000, -2.999999999999999556 ) ) ;
#1254 = CARTESIAN_POINT ( 'NONE',  ( 0.000000000000000000, 76.00000000000000000, 0.000000000000000000 ) ) ;
#1255 = CARTESIAN_POINT ( 'NONE',  ( -2.324088772396477476E-15, -29.68750000000000000, -5.250000000000000000 ) ) ;
#1256 = DIRECTION ( 'NONE',  ( 0.000000000000000000, 0.000000000000000000, 1.000000000000000000 ) ) ;
#1257 = CONTEXT_DEPENDENT_SHAPE_REPRESENTATION ( #7661, #9053 ) ;
#1258 = CARTESIAN_POINT ( 'NONE',  ( -3.807688866302469071E-16, -29.39062499965860198, -6.218427825808274356 ) ) ;
#1259 = CARTESIAN_POINT ( 'NONE',  ( 3.492485675378536047, -4.149340926099361226, 1.467888652719046672 ) ) ;
#1260 = CARTESIAN_POINT ( 'NONE',  ( -1.406733260263391960, -27.94866454968462932, 5.250000000000000000 ) ) ;
#1261 = CARTESIAN_POINT ( 'NONE',  ( 2.692658234375002735, -27.27604166632526628, 4.663820869356205101 ) ) ;
#1262 = CARTESIAN_POINT ( 'NONE',  ( 4.000000000000000000, -5.350659073900637885, -0.01814118441313441674 ) ) ;
#1263 = CARTESIAN_POINT ( 'NONE',  ( 0.000000000000000000, -27.00000000000000000, 0.000000000000000000 ) ) ;
#1264 = FACE_OUTER_BOUND ( 'NONE', #5853, .T. ) ;
#1265 = EDGE_CURVE ( 'NONE', #2260, #2834, #6581, .T. ) ;
#1266 = ORIENTED_EDGE ( 'NONE', *, *, #4371, .F. ) ;
#1267 = CARTESIAN_POINT ( 'NONE',  ( -5.249999999999999112, -28.22916666666666430, 3.031088913245538308 ) ) ;
#1268 = APPLICATION_CONTEXT ( 'automotive_design' ) ;
#1269 = CARTESIAN_POINT ( 'NONE',  ( -5.114683531250001636, -27.46354166700806587, 2.952963913586931444 ) ) ;
#1270 = CARTESIAN_POINT ( 'NONE',  ( 3.500000000000000000, -7.449340926099361937, 0.01814118441321387054 ) ) ;
#1271 = DIRECTION ( 'NONE',  ( -0.000000000000000000, -1.000000000000000000, -0.000000000000000000 ) ) ;
#1272 = CARTESIAN_POINT ( 'NONE',  ( 3.712013335537174572E-16, -29.93749999999999645, -6.062177826491070398 ) ) ;
#1273 = DIRECTION ( 'NONE',  ( 0.000000000000000000, -1.000000000000000000, 0.000000000000000000 ) ) ;
#1274 = CARTESIAN_POINT ( 'NONE',  ( -2.557341765625002594, -29.00520833367473017, 4.429445870380399164 ) ) ;
#1275 = CARTESIAN_POINT ( 'NONE',  ( -2.557341765625002594, -29.50520833367473017, 4.429445870380399164 ) ) ;
#1276 = CYLINDRICAL_SURFACE ( 'NONE', #8589, 5.250000000000000000 ) ;
#1277 = CARTESIAN_POINT ( 'NONE',  ( -5.250000000000000000, -29.45833333265053611, -3.031088913245534755 ) ) ;
#1278 = CARTESIAN_POINT ( 'NONE',  ( 5.385316468750000141, -29.98437499965859843, -6.595110575850215044E-16 ) ) ;
#1279 = FACE_OUTER_BOUND ( 'NONE', #5439, .T. ) ;
#1280 = CARTESIAN_POINT ( 'NONE',  ( 0.01814118441321408565, -1.449340926099361271, -3.500000000000000000 ) ) ;
#1281 = CARTESIAN_POINT ( 'NONE',  ( 1.431606283892619125, -2.349340926099361848, 3.507514324621464397 ) ) ;
#1282 = EDGE_LOOP ( 'NONE', ( #7453, #8242, #8885, #677 ) ) ;
#1283 = CARTESIAN_POINT ( 'NONE',  ( 5.250000000000000000, -29.12499999999999645, -6.429395695523604153E-16 ) ) ;
#1284 = CARTESIAN_POINT ( 'NONE',  ( 5.250000000000000000, -27.26041666734946034, -3.031088913245534755 ) ) ;
#1285 = CARTESIAN_POINT ( 'NONE',  ( 1.142306659890740623E-15, -29.54687499965859843, 6.218427825808274356 ) ) ;
#1286 = VERTEX_POINT ( 'NONE', #30 ) ;
#1287 = CARTESIAN_POINT ( 'NONE',  ( 5.385316468750000141, -28.95312499965860198, -6.595110575850215044E-16 ) ) ;
#1288 = CARTESIAN_POINT ( 'NONE',  ( 3.492485675378566690, -0.6506590739006391511, -1.467888652718972287 ) ) ;
#1289 = DIRECTION ( 'NONE',  ( 0.000000000000000000, 0.000000000000000000, 1.000000000000000000 ) ) ;
#1290 = ADVANCED_FACE ( 'NONE', ( #2880 ), #5743, .F. ) ;
#1291 =( BOUNDED_CURVE ( )  B_SPLINE_CURVE ( 2, ( #2841, #2089, #2795, #8507, #7762, #34, #601, #6972, #4914 ),
 .UNSPECIFIED., .F., .F. ) 
 B_SPLINE_CURVE_WITH_KNOTS ( ( 3, 2, 2, 2, 3 ),
 ( 0.4791666666666666852, 0.4861111111111111049, 0.5000000000000000000, 0.5138888888888888395, 0.5208333333333333703 ),
 .UNSPECIFIED. ) 
 CURVE ( )  GEOMETRIC_REPRESENTATION_ITEM ( )  RATIONAL_B_SPLINE_CURVE ( ( 0.9330127018922194093, 0.9330127018922196314, 1.000000000000000000, 0.8660254037844387076, 1.000000000000000000, 0.8660254037844387076, 1.000000000000000000, 0.9330127018922187432, 0.9330127018922192983 ) ) 
 REPRESENTATION_ITEM ( '' )  );
#1292 = CARTESIAN_POINT ( 'NONE',  ( -1.975475456537005874E-15, -28.31249999999999645, 5.250000000000000000 ) ) ;
#1293 = CARTESIAN_POINT ( 'NONE',  ( -3.500000000000000000, -6.649340926099361226, -0.01814118441321344033 ) ) ;
#1294 = CARTESIAN_POINT ( 'NONE',  ( -5.114683531250000748, -28.96354166700807298, 2.952963913586931888 ) ) ;
#1295 = CARTESIAN_POINT ( 'NONE',  ( 0.000000000000000000, -27.00000000000000000, 0.000000000000000000 ) ) ;
#1296 = CARTESIAN_POINT ( 'NONE',  ( 3.673940397442060361E-16, 1.000000000000000888, 3.000000000000000444 ) ) ;
#1297 = CARTESIAN_POINT ( 'NONE',  ( 3.507514324621465285, -4.349340926099361404, -1.431606283892619125 ) ) ;
#1298 = DIRECTION ( 'NONE',  ( 0.000000000000000000, 0.000000000000000000, 1.000000000000000000 ) ) ;
#1299 = COLOUR_RGB ( '',0.8941176470588234615, 0.8941176470588234615, 0.8941176470588234615 ) ;
#1300 = CARTESIAN_POINT ( 'NONE',  ( -5.385316468750000141, -27.35937499965860198, 0.000000000000000000 ) ) ;
#1301 = CARTESIAN_POINT ( 'NONE',  ( -2.841254879263473310, -1.150659073900638374, -2.815599370228907716 ) ) ;
#1302 = CARTESIAN_POINT ( 'NONE',  ( -5.250000000000000888, -27.10416666666666430, 3.031088913245532979 ) ) ;
#1303 = DIRECTION ( 'NONE',  ( 0.000000000000000000, 0.000000000000000000, -1.000000000000000000 ) ) ;
#1304 = PRESENTATION_LAYER_ASSIGNMENT (  '', '', ( #2499 ) ) ;
#1305 = ORIENTED_EDGE ( 'NONE', *, *, #4401, .F. ) ;
#1306 = CARTESIAN_POINT ( 'NONE',  ( -5.250000000000000000, -28.77083333333333215, -3.031088913245534755 ) ) ;
#1307 = EDGE_CURVE ( 'NONE', #6715, #7860, #2924, .T. ) ;
#1308 = CARTESIAN_POINT ( 'NONE',  ( -5.114683531250000748, -27.50520833367473017, -2.952963913586935440 ) ) ;
#1309 = CARTESIAN_POINT ( 'NONE',  ( -1.224499502706140497, -1.650659073900639484, 3.007514324621436863 ) ) ;
#1310 = CARTESIAN_POINT ( 'NONE',  ( -5.114683531250000748, -27.52604166700806587, 2.952963913586931888 ) ) ;
#1311 = CARTESIAN_POINT ( 'NONE',  ( 6.972266317189433020E-16, -27.93749999999999289, -5.250000000000000000 ) ) ;
#1312 = DIRECTION ( 'NONE',  ( -0.000000000000000000, -1.000000000000000000, -0.000000000000000000 ) ) ;
#1313 = CARTESIAN_POINT ( 'NONE',  ( 5.114683531249998971, -28.94270833367473017, 2.952963913586936329 ) ) ;
#1314 = FILL_AREA_STYLE ('',( #8394 ) ) ;
#1315 = AXIS2_PLACEMENT_3D ( 'NONE', #2177, #2930, #80 ) ;
#1316 = CARTESIAN_POINT ( 'NONE',  ( -1.084901341431563923E-15, -28.48437500034139802, 5.905927827173866440 ) ) ;
#1317 = CARTESIAN_POINT ( 'NONE',  ( 6.429395695523604153E-16, -30.00000000000000000, -5.250000000000000000 ) ) ;
#1318 = CARTESIAN_POINT ( 'NONE',  ( -3.712013335537174572E-16, -29.49999999931720041, -6.062177826491070398 ) ) ;
#1319 = CARTESIAN_POINT ( 'NONE',  ( -3.500000000000000000, -0.2493409260993610654, -0.01814118441321344033 ) ) ;
#1320 = CARTESIAN_POINT ( 'NONE',  ( -2.324088772396477476E-15, -29.46875000068279959, -5.250000000000000000 ) ) ;
#1321 = CARTESIAN_POINT ( 'NONE',  ( 6.972266317189434006E-16, -27.24999999931720751, -5.250000000000000000 ) ) ;
#1322 = CARTESIAN_POINT ( 'NONE',  ( -3.507514324621464397, -5.149340926099360338, 1.431606283892619347 ) ) ;
#1323 = CARTESIAN_POINT ( 'NONE',  ( -2.487701488670255312, -0.4493409260993610488, 2.462045979635577808 ) ) ;
#1324 = ORIENTED_EDGE ( 'NONE', *, *, #8892, .T. ) ;
#1325 = VECTOR ( 'NONE', #2363, 1000.000000000000000 ) ;
#1326 = LINE ( 'NONE', #2780, #1633 ) ;
#1327 = CARTESIAN_POINT ( 'NONE',  ( 2.557341765625000818, -29.31770833367473017, -4.429445870380400052 ) ) ;
#1328 = CARTESIAN_POINT ( 'NONE',  ( 5.385316468749999252, -29.96354166632526628, -3.109213912904139399 ) ) ;
#1329 = EDGE_CURVE ( 'NONE', #2527, #7225, #4224, .T. ) ;
#1330 = ORIENTED_EDGE ( 'NONE', *, *, #8424, .F. ) ;
#1331 = CARTESIAN_POINT ( 'NONE',  ( 2.692658234375002735, -29.99479166632526628, 4.663820869356205101 ) ) ;
#1332 = CARTESIAN_POINT ( 'NONE',  ( 2.487701488670203354, -5.150659073900639484, 2.462045979635629323 ) ) ;
#1333 = DIRECTION ( 'NONE',  ( -0.000000000000000000, -1.000000000000000000, -0.000000000000000000 ) ) ;
#1334 = CIRCLE ( 'NONE', #7748, 1.500000000000000222 ) ;
#1335 = EDGE_CURVE ( 'NONE', #8226, #5826, #3482, .T. ) ;
#1336 = DIRECTION ( 'NONE',  ( 0.000000000000000000, 1.000000000000000000, 0.000000000000000000 ) ) ;
#1337 = CARTESIAN_POINT ( 'NONE',  ( 0.000000000000000000, -53.00000000000000000, 0.000000000000000000 ) ) ;
#1338 = AXIS2_PLACEMENT_3D ( 'NONE', #873, #178, #3771 ) ;
#1339 = PRODUCT_DEFINITION_CONTEXT ( 'detailed design', #4961, 'design' ) ;
#1340 = CARTESIAN_POINT ( 'NONE',  ( 1.406733260263393737, -27.26116454900182973, -5.250000000000000000 ) ) ;
#1341 = CARTESIAN_POINT ( 'NONE',  ( -5.114683531250000748, -27.96354166700806587, 2.952963913586931888 ) ) ;
#1342 = FACE_OUTER_BOUND ( 'NONE', #5979, .T. ) ;
#1343 = AXIS2_PLACEMENT_3D ( 'NONE', #8806, #6806, #1036 ) ;
#1344 = CARTESIAN_POINT ( 'NONE',  ( 5.249999999999997335, -29.05208333401613174, 3.031088913245538308 ) ) ;
#1345 = CARTESIAN_POINT ( 'NONE',  ( -2.992485675378538268, -3.349340926099362292, -1.260781871532495879 ) ) ;
#1346 =( BOUNDED_CURVE ( )  B_SPLINE_CURVE ( 2, ( #6435, #2875, #1377, #3478, #5606, #5565, #3520, #6305, #9097 ),
 .UNSPECIFIED., .F., .F. ) 
 B_SPLINE_CURVE_WITH_KNOTS ( ( 3, 2, 2, 2, 3 ),
 ( 0.9375000000000000000, 0.9444444444444444198, 0.9583333333333333703, 0.9722222222222222099, 0.9791666666666667407 ),
 .UNSPECIFIED. ) 
 CURVE ( )  GEOMETRIC_REPRESENTATION_ITEM ( )  RATIONAL_B_SPLINE_CURVE ( ( 0.9330127018922194093, 0.9330127018922194093, 1.000000000000000000, 0.8660254037844387076, 1.000000000000000000, 0.8660254037844387076, 1.000000000000000000, 0.9330127018922187432, 0.9330127018922192983 ) ) 
 REPRESENTATION_ITEM ( '' )  );
#1347 = CARTESIAN_POINT ( 'NONE',  ( 2.625000000000002220, -28.66666666666666785, 4.546633369868302132 ) ) ;
#1348 = CARTESIAN_POINT ( 'NONE',  ( 5.385316468750000141, -29.70312499965859843, -6.595110575850215044E-16 ) ) ;
#1349 = CARTESIAN_POINT ( 'NONE',  ( -1.638713065079245634, -3.250659073900639129, 4.007514324621432422 ) ) ;
#1350 = CARTESIAN_POINT ( 'NONE',  ( 1.185285273922203525E-14, -28.93749999999999645, -5.250000000000000000 ) ) ;
#1351 = AXIS2_PLACEMENT_3D ( 'NONE', #2624, #3965, #1966 ) ;
#1352 = CYLINDRICAL_SURFACE ( 'NONE', #1343, 3.999999999999999112 ) ;
#1353 = ORIENTED_EDGE ( 'NONE', *, *, #3526, .T. ) ;
#1354 = CARTESIAN_POINT ( 'NONE',  ( 2.692658234375002735, -27.24479166632526628, 4.663820869356205101 ) ) ;
#1355 = ORIENTED_EDGE ( 'NONE', *, *, #173, .F. ) ;
#1356 = CARTESIAN_POINT ( 'NONE',  ( -1.084901341431563726E-15, -27.67187500034140157, 5.905927827173866440 ) ) ;
#1357 = CARTESIAN_POINT ( 'NONE',  ( -2.992485675378538268, -6.549340926099361582, -1.260781871532495879 ) ) ;
#1358 = CARTESIAN_POINT ( 'NONE',  ( 5.114683531249998971, -27.19270833367473017, 2.952963913586936329 ) ) ;
#1359 = DIRECTION ( 'NONE',  ( 0.000000000000000000, 1.000000000000000000, 0.000000000000000000 ) ) ;
#1360 = ADVANCED_FACE ( 'NONE', ( #4178, #2747 ), #7806, .F. ) ;
#1361 = CARTESIAN_POINT ( 'NONE',  ( -1.084901341431563726E-15, -29.73437500034140513, 5.905927827173866440 ) ) ;
#1362 = DIRECTION ( 'NONE',  ( 0.000000000000000000, -1.000000000000000000, 0.000000000000000000 ) ) ;
#1363 = CARTESIAN_POINT ( 'NONE',  ( 5.114683531250000748, -27.92187500034139802, 0.000000000000000000 ) ) ;
#1364 = CARTESIAN_POINT ( 'NONE',  ( -5.250000000000000000, -29.62500000000000000, -6.429395695523604153E-16 ) ) ;
#1365 = CARTESIAN_POINT ( 'NONE',  ( 5.250000000000000000, -29.81249999931720041, -6.429395695523604153E-16 ) ) ;
#1366 = CARTESIAN_POINT ( 'NONE',  ( 0.000000000000000000, 74.00000000000001421, 0.000000000000000000 ) ) ;
#1367 = DIRECTION ( 'NONE',  ( 0.000000000000000000, 1.000000000000000000, 0.000000000000000000 ) ) ;
#1368 = LINE ( 'NONE', #9131, #1829 ) ;
#1369 = CARTESIAN_POINT ( 'NONE',  ( 1.431606283892619125, -3.949340926099361049, 3.507514324621464397 ) ) ;
#1370 = CARTESIAN_POINT ( 'NONE',  ( -0.01814118441321365544, -7.049340926099361582, 3.500000000000000000 ) ) ;
#1371 = EDGE_LOOP ( 'NONE', ( #5607, #6567, #6671, #3159 ) ) ;
#1372 = CARTESIAN_POINT ( 'NONE',  ( 0.000000000000000000, 79.00000000000001421, -4.000000000000000000 ) ) ;
#1373 = CARTESIAN_POINT ( 'NONE',  ( -5.114683531249999859, -29.25520833367473017, -2.952963913586935440 ) ) ;
#1374 = VERTEX_POINT ( 'NONE', #9144 ) ;
#1375 = CARTESIAN_POINT ( 'NONE',  ( -5.385316468750000141, -29.07812499965860198, 0.000000000000000000 ) ) ;
#1376 = CARTESIAN_POINT ( 'NONE',  ( -1.467888652718973619, -4.250659073900639129, -3.492485675378565801 ) ) ;
#1377 = CARTESIAN_POINT ( 'NONE',  ( -2.624999999999998668, -27.16666666666666430, -4.546633369868303021 ) ) ;
#1378 = VERTEX_POINT ( 'NONE', #8543 ) ;
#1379 = CARTESIAN_POINT ( 'NONE',  ( -2.624999999999996891, -28.95833333333333215, 4.546633369868304797 ) ) ;
#1380 = CARTESIAN_POINT ( 'NONE',  ( 0.000000000000000000, 76.00000000000000000, 0.000000000000000000 ) ) ;
#1381 = VECTOR ( 'NONE', #1273, 1000.000000000000000 ) ;
#1382 = CARTESIAN_POINT ( 'NONE',  ( 5.114683531250000748, -28.35937500034139447, 0.000000000000000000 ) ) ;
#1383 = CARTESIAN_POINT ( 'NONE',  ( 6.429395695523604153E-16, -30.00000000000000000, -5.250000000000000000 ) ) ;
#1384 = CARTESIAN_POINT ( 'NONE',  ( 2.624999999999998668, -27.77083333265053255, -4.546633369868303021 ) ) ;
#1385 = CARTESIAN_POINT ( 'NONE',  ( -0.01814118441320841310, -5.449340926099361937, 3.000000000000000444 ) ) ;
#1386 = ADVANCED_FACE ( 'NONE', ( #5610 ), #2170, .F. ) ;
#1387 = DIRECTION ( 'NONE',  ( 0.000000000000000000, -0.000000000000000000, -1.000000000000000000 ) ) ;
#1388 = AXIS2_PLACEMENT_3D ( 'NONE', #217, #4363, #5844 ) ;
#1389 = CARTESIAN_POINT ( 'NONE',  ( 2.692658234375002735, -29.74479166632526983, 4.663820869356205101 ) ) ;
#1390 = CARTESIAN_POINT ( 'NONE',  ( 0.01814118441313467001, -0.1506590739006384849, 4.000000000000000000 ) ) ;
#1391 = AXIS2_PLACEMENT_3D ( 'NONE', #2767, #1359, #9161 ) ;
#1392 = CARTESIAN_POINT ( 'NONE',  ( 1.000000000000000000, -29.00000000000000355, 1.118033988749894680 ) ) ;
#1393 = LINE ( 'NONE', #9153, #2840 ) ;
#1394 =( BOUNDED_CURVE ( )  B_SPLINE_CURVE ( 2, ( #4872, #2888, #8549, #6490, #2046, #5750, #3489, #2797, #6356 ),
 .UNSPECIFIED., .F., .F. ) 
 B_SPLINE_CURVE_WITH_KNOTS ( ( 3, 2, 2, 2, 3 ),
 ( 0.5208333333333332593, 0.5277777777777777901, 0.5416666666666666297, 0.5555555555555555802, 0.5625000000000000000 ),
 .UNSPECIFIED. ) 
 CURVE ( )  GEOMETRIC_REPRESENTATION_ITEM ( )  RATIONAL_B_SPLINE_CURVE ( ( 0.9330127018922192983, 0.9330127018922187432, 1.000000000000000000, 0.8660254037844387076, 1.000000000000000000, 0.8660254037844387076, 1.000000000000000000, 0.9330127018922194093, 0.9330127018922194093 ) ) 
 REPRESENTATION_ITEM ( '' )  );
#1395 = ORIENTED_EDGE ( 'NONE', *, *, #4836, .T. ) ;
#1396 = SURFACE_SIDE_STYLE ('',( #4281 ) ) ;
#1397 = CARTESIAN_POINT ( 'NONE',  ( 5.250000000000000888, -29.64583333333333215, 3.031088913245532979 ) ) ;
#1398 = EDGE_CURVE ( 'NONE', #6849, #8000, #8214, .T. ) ;
#1399 = CARTESIAN_POINT ( 'NONE',  ( -5.114683531250000748, -27.23437500034139802, -6.263680815196995234E-16 ) ) ;
#1400 = CARTESIAN_POINT ( 'NONE',  ( 0.01814118441320878086, -7.849340926099363180, -3.000000000000000444 ) ) ;
#1401 = CARTESIAN_POINT ( 'NONE',  ( 3.712013335537174572E-16, -28.68749999999999645, -6.062177826491070398 ) ) ;
#1402 = CARTESIAN_POINT ( 'NONE',  ( 0.000000000000000000, -27.00000000000000000, 0.000000000000000000 ) ) ;
#1403 = EDGE_CURVE ( 'NONE', #6870, #7184, #6991, .T. ) ;
#1404 = CARTESIAN_POINT ( 'NONE',  ( -2.557341765624999042, -29.08854166700806587, -4.429445870380400052 ) ) ;
#1405 = SURFACE_STYLE_USAGE ( .BOTH. , #618 ) ;
#1406 = CARTESIAN_POINT ( 'NONE',  ( 3.616337804771879580E-16, -27.10937500034139802, -5.905927827173866440 ) ) ;
#1407 = CARTESIAN_POINT ( 'NONE',  ( -2.624999999999996891, -29.20833333333333215, 4.546633369868304797 ) ) ;
#1408 = CARTESIAN_POINT ( 'NONE',  ( 5.250000000000000000, -29.54166666598386826, -3.031088913245536531 ) ) ;
#1409 = PLANE ( 'NONE',  #344 ) ;
#1410 = CARTESIAN_POINT ( 'NONE',  ( -1.931223450958591048, -1.125130374610754074E-16, 2.930832316995867437 ) ) ;
#1411 = CARTESIAN_POINT ( 'NONE',  ( -5.385316468749998364, -30.08854166632526983, 3.109213912904140287 ) ) ;
#1412 = CARTESIAN_POINT ( 'NONE',  ( 6.972266317189433020E-16, -29.71875000068279249, -5.250000000000000000 ) ) ;
#1413 = ORIENTED_EDGE ( 'NONE', *, *, #4803, .T. ) ;
#1414 = CARTESIAN_POINT ( 'NONE',  ( 2.161402558328724325E-14, -29.74999999931720396, -5.250000000000000000 ) ) ;
#1415 = CARTESIAN_POINT ( 'NONE',  ( 3.616337804771879580E-16, -29.54687500034139802, -5.905927827173866440 ) ) ;
#1416 =( BOUNDED_CURVE ( )  B_SPLINE_CURVE ( 2, ( #1311, #1432, #7906, #5667, #2141, #5805, #4415, #828, #44 ),
 .UNSPECIFIED., .F., .T. ) 
 B_SPLINE_CURVE_WITH_KNOTS ( ( 3, 2, 2, 2, 3 ),
 ( 0.6875000000000000000, 0.6944444444444444198, 0.7083333333333333703, 0.7222222222222222099, 0.7291666666666667407 ),
 .UNSPECIFIED. ) 
 CURVE ( )  GEOMETRIC_REPRESENTATION_ITEM ( )  RATIONAL_B_SPLINE_CURVE ( ( 0.9330127018922194093, 0.9330127018922194093, 1.000000000000000000, 0.8660254037844387076, 1.000000000000000000, 0.8660254037844387076, 1.000000000000000000, 0.9330127018922187432, 0.9330127018922192983 ) ) 
 REPRESENTATION_ITEM ( '' )  );
#1417 = ORIENTED_EDGE ( 'NONE', *, *, #5588, .F. ) ;
#1418 = CARTESIAN_POINT ( 'NONE',  ( -2.692658234374996518, -29.78645833299193413, 4.663820869356208654 ) ) ;
#1419 = CARTESIAN_POINT ( 'NONE',  ( 3.500000000000000000, -5.350659073900638774, -0.01814118441313969030 ) ) ;
#1420 = DIRECTION ( 'NONE',  ( -0.000000000000000000, -0.000000000000000000, 1.000000000000000000 ) ) ;
#1421 = ORIENTED_EDGE ( 'NONE', *, *, #9098, .F. ) ;
#1422 = CARTESIAN_POINT ( 'NONE',  ( 2.161402558328724325E-14, -29.49999999931720396, -5.250000000000000000 ) ) ;
#1423 = CARTESIAN_POINT ( 'NONE',  ( 4.898587196589412829E-16, 81.00000000000001421, 4.000000000000000000 ) ) ;
#1424 = CARTESIAN_POINT ( 'NONE',  ( 2.624999999999996891, -27.82291666734946389, 4.546633369868304797 ) ) ;
#1425 = CARTESIAN_POINT ( 'NONE',  ( 5.114683531249998971, -28.38020833367473372, 2.952963913586936329 ) ) ;
#1426 = CARTESIAN_POINT ( 'NONE',  ( 2.625000000000000444, -27.48958333401612819, -4.546633369868303021 ) ) ;
#1427 = CARTESIAN_POINT ( 'NONE',  ( -2.624999999999998668, -28.94791666734946389, -4.546633369868303021 ) ) ;
#1428 = CARTESIAN_POINT ( 'NONE',  ( -1.224499502706077880, -4.749340926099361759, -3.007514324621463064 ) ) ;
#1429 = CARTESIAN_POINT ( 'NONE',  ( 2.161402558328724325E-14, -29.31250000000000000, -5.250000000000000000 ) ) ;
#1430 = CARTESIAN_POINT ( 'NONE',  ( 1.142306659890740623E-15, -28.04687499965860198, 6.218427825808274356 ) ) ;
#1431 = CARTESIAN_POINT ( 'NONE',  ( -0.01814118441313417734, -0.9506590739006385293, -4.000000000000000000 ) ) ;
#1432 = CARTESIAN_POINT ( 'NONE',  ( -1.406733260263393293, -27.92633545031536713, -5.250000000000000000 ) ) ;
#1433 = PRODUCT ( 'top sleeve', 'top sleeve', '', ( #6229 ) ) ;
#1434 = VERTEX_POINT ( 'NONE', #7055 ) ;
#1435 = CARTESIAN_POINT ( 'NONE',  ( -2.692658234375000514, -27.36979166632526628, -4.663820869356205989 ) ) ;
#1436 = ADVANCED_FACE ( 'NONE', ( #679 ), #3525, .F. ) ;
#1437 = CARTESIAN_POINT ( 'NONE',  ( -5.114683531250000748, -26.98437500034139802, -6.263680815196995234E-16 ) ) ;
#1438 = CARTESIAN_POINT ( 'NONE',  ( -2.108492589042306964, -8.049340926099361582, -2.134148098076978251 ) ) ;
#1439 = VERTEX_POINT ( 'NONE', #3570 ) ;
#1440 = CARTESIAN_POINT ( 'NONE',  ( 5.249999999999999112, -29.02083333333333570, 3.031088913245538308 ) ) ;
#1441 = DIRECTION ( 'NONE',  ( 0.000000000000000000, 0.000000000000000000, 1.000000000000000000 ) ) ;
#1442 = EDGE_CURVE ( 'NONE', #1286, #7860, #7941, .T. ) ;
#1443 = CARTESIAN_POINT ( 'NONE',  ( -5.114683531250001636, -29.52604166700806232, 2.952963913586931444 ) ) ;
#1444 = EDGE_CURVE ( 'NONE', #7933, #3802, #2311, .T. ) ;
#1445 = CARTESIAN_POINT ( 'NONE',  ( -5.114683531249999859, -27.81770833367473017, -2.952963913586935440 ) ) ;
#1446 =( GEOMETRIC_REPRESENTATION_CONTEXT ( 3 ) GLOBAL_UNCERTAINTY_ASSIGNED_CONTEXT ( ( #8127 ) ) GLOBAL_UNIT_ASSIGNED_CONTEXT ( ( #6548, #7300, #5480 ) ) REPRESENTATION_CONTEXT ( 'NONE', 'WORKASPACE' ) );
#1447 = CARTESIAN_POINT ( 'NONE',  ( -5.249999999999999112, -29.66666666598386826, 3.031088913245538308 ) ) ;
#1448 = CARTESIAN_POINT ( 'NONE',  ( -1.000000000000000000, -35.00000000000000000, -2.880243826144208708 ) ) ;
#1449 = CARTESIAN_POINT ( 'NONE',  ( -3.709488398121285169, -3.053917841153453545E-13, 0.6142436145054751551 ) ) ;
#1450 = FACE_OUTER_BOUND ( 'NONE', #5236, .T. ) ;
#1451 = CARTESIAN_POINT ( 'NONE',  ( 0.000000000000000000, -30.00000000000000000, 0.000000000000000000 ) ) ;
#1452 = SURFACE_STYLE_USAGE ( .BOTH. , #844 ) ;
#1453 = EDGE_LOOP ( 'NONE', ( #2480, #5936, #1395, #6149 ) ) ;
#1454 = CARTESIAN_POINT ( 'NONE',  ( 2.462045979635629767, -7.150659073900639484, -2.487701488670203354 ) ) ;
#1455 = CARTESIAN_POINT ( 'NONE',  ( 1.975475456537005874E-15, -29.62499999931719685, 5.250000000000000000 ) ) ;
#1456 = CARTESIAN_POINT ( 'NONE',  ( 5.249999999999999112, -26.80208333401613174, 3.031088913245538308 ) ) ;
#1457 = EDGE_LOOP ( 'NONE', ( #8075, #3517, #4280, #8793 ) ) ;
#1458 = ORIENTED_EDGE ( 'NONE', *, *, #2475, .T. ) ;
#1459 = CARTESIAN_POINT ( 'NONE',  ( -3.807688866302469071E-16, -29.39062499965859843, -6.218427825808274356 ) ) ;
#1460 = CARTESIAN_POINT ( 'NONE',  ( 1.467888652718972731, -5.050659073900638063, 3.492485675378566246 ) ) ;
#1461 = FACE_OUTER_BOUND ( 'NONE', #6409, .T. ) ;
#1462 = AXIS2_PLACEMENT_3D ( 'NONE', #3623, #6446, #2975 ) ;
#1463 = ORIENTED_EDGE ( 'NONE', *, *, #8661, .F. ) ;
#1464 = EDGE_CURVE ( 'NONE', #6101, #3013, #5044, .T. ) ;
#1465 = LINE ( 'NONE', #5884, #5657 ) ;
#1466 = CARTESIAN_POINT ( 'NONE',  ( 1.000000000000000000, -35.00000000000000000, -2.880243826144208708 ) ) ;
#1467 =( BOUNDED_CURVE ( )  B_SPLINE_CURVE ( 2, ( #5656, #1340, #7056, #2085, #9185, #772, #5744, #7807, #3659 ),
 .UNSPECIFIED., .F., .T. ) 
 B_SPLINE_CURVE_WITH_KNOTS ( ( 3, 2, 2, 2, 3 ),
 ( 0.02083333333333333565, 0.02777777777777777624, 0.04166666666666666435, 0.05555555555555555247, 0.06250000000000000000 ),
 .UNSPECIFIED. ) 
 CURVE ( )  GEOMETRIC_REPRESENTATION_ITEM ( )  RATIONAL_B_SPLINE_CURVE ( ( 0.9330127018922194093, 0.9330127018922194093, 1.000000000000000000, 0.8660254037844387076, 1.000000000000000000, 0.8660254037844387076, 1.000000000000000000, 0.9330127018922194093, 0.9330127018922194093 ) ) 
 REPRESENTATION_ITEM ( '' )  );
#1468 = ADVANCED_FACE ( 'NONE', ( #3803 ), #817, .T. ) ;
#1469 = DIRECTION ( 'NONE',  ( 0.000000000000000000, 0.000000000000000000, -1.000000000000000000 ) ) ;
#1470 = VECTOR ( 'NONE', #8499, 1000.000000000000000 ) ;
#1471 = CARTESIAN_POINT ( 'NONE',  ( -5.114683531249999859, -29.00520833367473017, -2.952963913586935440 ) ) ;
#1472 = DIRECTION ( 'NONE',  ( 0.000000000000000000, 1.000000000000000000, 0.000000000000000000 ) ) ;
#1473 = CARTESIAN_POINT ( 'NONE',  ( 0.000000000000000000, 81.00000000000001421, 0.000000000000000000 ) ) ;
#1474 = CARTESIAN_POINT ( 'NONE',  ( -3.007514324621463508, -5.149340926099361226, 1.224499502706077658 ) ) ;
#1475 = DIRECTION ( 'NONE',  ( 0.000000000000000000, 1.000000000000000000, 0.000000000000000000 ) ) ;
#1476 = CARTESIAN_POINT ( 'NONE',  ( -5.385316468750001029, -28.63020833299193413, -3.109213912904136734 ) ) ;
#1477 = CARTESIAN_POINT ( 'NONE',  ( -4.007514324621431534, -7.650659073900639484, -1.638713065079248521 ) ) ;
#1478 = CIRCLE ( 'NONE', #6676, 5.250000000000000000 ) ;
#1479 = CLOSED_SHELL ( 'NONE', ( #4412, #3247, #2822, #5525, #9073, #2667, #4256, #5038, #4493, #35, #5330, #3737 ) ) ;
#1480 = CARTESIAN_POINT ( 'NONE',  ( -2.625000000000002220, -27.61458333401612819, 4.546633369868302132 ) ) ;
#1481 = AXIS2_PLACEMENT_3D ( 'NONE', #8184, #5149, #1012 ) ;
#1482 = ORIENTED_EDGE ( 'NONE', *, *, #9169, .F. ) ;
#1483 = CARTESIAN_POINT ( 'NONE',  ( 5.250000000000000000, -29.85416666666667140, -3.031088913245536531 ) ) ;
#1484 = ORIENTED_EDGE ( 'NONE', *, *, #1125, .F. ) ;
#1485 = CARTESIAN_POINT ( 'NONE',  ( 2.324088772396477476E-15, -27.31250000000000000, -5.250000000000000000 ) ) ;
#1486 = CARTESIAN_POINT ( 'NONE',  ( -2.108492589042306964, -6.449340926099361049, -2.134148098076978251 ) ) ;
#1487 = AXIS2_PLACEMENT_3D ( 'NONE', #3149, #8300, #8894 ) ;
#1488 = ORIENTED_EDGE ( 'NONE', *, *, #2428, .F. ) ;
#1489 = CARTESIAN_POINT ( 'NONE',  ( 5.250000000000000000, -28.74999999999999645, 0.000000000000000000 ) ) ;
#1490 = DIRECTION ( 'NONE',  ( 0.000000000000000000, 1.000000000000000000, 0.000000000000000000 ) ) ;
#1491 = CARTESIAN_POINT ( 'NONE',  ( 2.557341765624996821, -27.96354166700806587, 4.429445870380401828 ) ) ;
#1492 = VECTOR ( 'NONE', #5566, 1000.000000000000114 ) ;
#1493 = CARTESIAN_POINT ( 'NONE',  ( -2.557341765625002594, -27.75520833367473017, 4.429445870380399164 ) ) ;
#1494 = CARTESIAN_POINT ( 'NONE',  ( -5.114683531250001636, -29.71354166700806232, 2.952963913586931444 ) ) ;
#1495 = DIRECTION ( 'NONE',  ( 0.000000000000000000, 1.000000000000000000, 0.000000000000000000 ) ) ;
#1496 = EDGE_CURVE ( 'NONE', #1166, #179, #8185, .T. ) ;
#1497 = DIRECTION ( 'NONE',  ( 0.000000000000000000, 0.000000000000000000, -1.000000000000000000 ) ) ;
#1498 = CARTESIAN_POINT ( 'NONE',  ( -1.000000000000000000, -35.00000000000000000, 2.880243826144208708 ) ) ;
#1499 = CARTESIAN_POINT ( 'NONE',  ( -5.250000000000000888, -29.63541666734946389, 3.031088913245533423 ) ) ;
#1500 = CARTESIAN_POINT ( 'NONE',  ( -3.500000000000000000, -6.649340926099361226, -0.01814118441321344033 ) ) ;
#1501 = ORIENTED_EDGE ( 'NONE', *, *, #851, .T. ) ;
#1502 = CARTESIAN_POINT ( 'NONE',  ( -2.624999999999998668, -28.69791666734946389, -4.546633369868303021 ) ) ;
#1503 = CARTESIAN_POINT ( 'NONE',  ( -5.250000000000000888, -29.35416666666666430, 3.031088913245533423 ) ) ;
#1504 = CARTESIAN_POINT ( 'NONE',  ( 5.114683531249998971, -28.88020833367473017, 2.952963913586936329 ) ) ;
#1505 = ORIENTED_EDGE ( 'NONE', *, *, #8954, .F. ) ;
#1506 = EDGE_LOOP ( 'NONE', ( #5687, #3390 ) ) ;
#1507 = CARTESIAN_POINT ( 'NONE',  ( 0.000000000000000000, -30.00000000000000000, 0.000000000000000000 ) ) ;
#1508 = EDGE_CURVE ( 'NONE', #3111, #3057, #6807, .T. ) ;
#1509 = CARTESIAN_POINT ( 'NONE',  ( 1.406733260263390628, -28.17633545031536357, 5.250000000000001776 ) ) ;
#1510 = CARTESIAN_POINT ( 'NONE',  ( -0.01814118441313947866, -4.150659073900639484, -3.500000000000000000 ) ) ;
#1511 = CARTESIAN_POINT ( 'NONE',  ( 6.972266317189433020E-16, -26.96875000068279249, -5.249999999999999112 ) ) ;
#1512 = ORIENTED_EDGE ( 'NONE', *, *, #6392, .T. ) ;
#1513 = CARTESIAN_POINT ( 'NONE',  ( -2.624999999999998668, -27.66666666666666430, -4.546633369868303021 ) ) ;
#1514 = CARTESIAN_POINT ( 'NONE',  ( -1.000000000000000000, -35.00000000000000000, -3.048902179152658931 ) ) ;
#1515 = CARTESIAN_POINT ( 'NONE',  ( 5.250000000000000888, -28.89583333333333215, 3.031088913245533423 ) ) ;
#1516 = UNCERTAINTY_MEASURE_WITH_UNIT (LENGTH_MEASURE( 1.000000000000000082E-05 ), #2714, 'distance_accuracy_value', 'NONE');
#1517 = CARTESIAN_POINT ( 'NONE',  ( 5.114683531249999859, -27.33854166700806232, -2.952963913586932776 ) ) ;
#1518 = CARTESIAN_POINT ( 'NONE',  ( 2.487701488670255756, -1.249340926099361093, -2.462045979635577364 ) ) ;
#1519 = CARTESIAN_POINT ( 'NONE',  ( -2.692658234375000514, -27.11979166632526628, -4.663820869356205989 ) ) ;
#1520 = CARTESIAN_POINT ( 'NONE',  ( -1.260781871532494103, -2.149340926099361226, 2.992485675378538712 ) ) ;
#1521 = CYLINDRICAL_SURFACE ( 'NONE', #2813, 5.750000000000000000 ) ;
#1522 = CARTESIAN_POINT ( 'NONE',  ( 5.385316468749999252, -28.71354166632526628, -3.109213912904139399 ) ) ;
#1523 = CARTESIAN_POINT ( 'NONE',  ( -0.01814118441313417734, -7.350659073900637885, -4.000000000000000000 ) ) ;
#1524 = VECTOR ( 'NONE', #7266, 1000.000000000000000 ) ;
#1525 = CARTESIAN_POINT ( 'NONE',  ( 0.000000000000000000, -9.000000000000001776, 0.000000000000000000 ) ) ;
#1526 = LINE ( 'NONE', #2181, #6846 ) ;
#1527 = DIRECTION ( 'NONE',  ( 0.000000000000000000, 1.000000000000000000, 0.000000000000000000 ) ) ;
#1528 = ORIENTED_EDGE ( 'NONE', *, *, #1120, .T. ) ;
#1529 = CIRCLE ( 'NONE', #2124, 6.250000000000000000 ) ;
#1530 = CARTESIAN_POINT ( 'NONE',  ( 5.385316468750001029, -27.22395833299193413, 3.109213912904135846 ) ) ;
#1531 =( GEOMETRIC_REPRESENTATION_CONTEXT ( 3 ) GLOBAL_UNCERTAINTY_ASSIGNED_CONTEXT ( ( #996 ) ) GLOBAL_UNIT_ASSIGNED_CONTEXT ( ( #5266, #3746, #3885 ) ) REPRESENTATION_CONTEXT ( 'NONE', 'WORKASPACE' ) );
#1532 = ORIENTED_EDGE ( 'NONE', *, *, #3503, .F. ) ;
#1533 = CARTESIAN_POINT ( 'NONE',  ( -5.249999999999999112, -27.27083333333333570, -3.031088913245534755 ) ) ;
#1534 = CARTESIAN_POINT ( 'NONE',  ( -2.108492589042352261, -3.150659073900639484, 2.134148098076933397 ) ) ;
#1535 = ORIENTED_EDGE ( 'NONE', *, *, #517, .F. ) ;
#1536 = CARTESIAN_POINT ( 'NONE',  ( -5.250000000000000000, -29.37500000000000000, -6.429395695523604153E-16 ) ) ;
#1537 = DIRECTION ( 'NONE',  ( 0.000000000000000000, 1.000000000000000000, 0.000000000000000000 ) ) ;
#1538 = EDGE_CURVE ( 'NONE', #813, #6454, #6058, .T. ) ;
#1539 = CIRCLE ( 'NONE', #1251, 4.000000000000000000 ) ;
#1540 = CARTESIAN_POINT ( 'NONE',  ( -5.114683531250001636, -27.77604166700806587, 2.952963913586931444 ) ) ;
#1541 = DIRECTION ( 'NONE',  ( 0.000000000000000000, 0.000000000000000000, 1.000000000000000000 ) ) ;
#1542 = CARTESIAN_POINT ( 'NONE',  ( 3.616337804771879580E-16, -28.10937500034140157, -5.905927827173866440 ) ) ;
#1543 = PRODUCT_DEFINITION ( 'UNKNOWN', '', #8579, #8974 ) ;
#1544 = CARTESIAN_POINT ( 'NONE',  ( 5.250000000000000000, -30.04166666598386826, -3.031088913245536531 ) ) ;
#1545 = CARTESIAN_POINT ( 'NONE',  ( -1.467888652719046449, -2.149340926099360782, 3.492485675378536047 ) ) ;
#1546 = CARTESIAN_POINT ( 'NONE',  ( 1.975475456537005874E-15, -27.87499999931720041, 5.249999999999999112 ) ) ;
#1547 = CARTESIAN_POINT ( 'NONE',  ( -1.975475456537005874E-15, -27.34375000068279249, 5.250000000000000000 ) ) ;
#1548 = CARTESIAN_POINT ( 'NONE',  ( -2.487701488670255312, -6.849340926099361404, 2.462045979635577808 ) ) ;
#1549 = FILL_AREA_STYLE ('',( #5774 ) ) ;
#1550 = VERTEX_POINT ( 'NONE', #4069 ) ;
#1551 = CARTESIAN_POINT ( 'NONE',  ( -0.01814118441313947866, -7.350659073900638774, -3.500000000000000000 ) ) ;
#1552 = CARTESIAN_POINT ( 'NONE',  ( 5.249999999999999112, -27.97916666666666430, -3.031088913245534755 ) ) ;
#1553 = CARTESIAN_POINT ( 'NONE',  ( 2.557341765625000818, -28.81770833367473017, -4.429445870380400052 ) ) ;
#1554 = ORIENTED_EDGE ( 'NONE', *, *, #6379, .F. ) ;
#1555 = ORIENTED_EDGE ( 'NONE', *, *, #1645, .F. ) ;
#1556 = DIRECTION ( 'NONE',  ( 0.000000000000000000, -1.000000000000000000, 0.000000000000000000 ) ) ;
#1557 = CARTESIAN_POINT ( 'NONE',  ( 5.250000000000000888, -28.14583333333333215, 3.031088913245533423 ) ) ;
#1558 = CARTESIAN_POINT ( 'NONE',  ( -2.841254879263473310, -5.950659073900640195, -2.815599370228907716 ) ) ;
#1559 = CARTESIAN_POINT ( 'NONE',  ( -2.033577675846918216E-14, -29.37499999931720396, 5.250000000000000888 ) ) ;
#1560 = EDGE_LOOP ( 'NONE', ( #8776, #8250, #6632, #1501 ) ) ;
#1561 = DIRECTION ( 'NONE',  ( 0.000000000000000000, 1.000000000000000000, 0.000000000000000000 ) ) ;
#1562 = CARTESIAN_POINT ( 'NONE',  ( 2.624999999999996891, -29.32291666734946034, 4.546633369868304797 ) ) ;
#1563 = CARTESIAN_POINT ( 'NONE',  ( 2.692658234375002735, -27.52604166632526628, 4.663820869356205101 ) ) ;
#1564 = CARTESIAN_POINT ( 'NONE',  ( 5.114683531249998971, -26.88020833367473017, 2.952963913586936329 ) ) ;
#1565 = CARTESIAN_POINT ( 'NONE',  ( 1.467888652719048226, -2.949340926099361493, -3.492485675378536047 ) ) ;
#1566 = DIRECTION ( 'NONE',  ( 0.000000000000000000, 0.000000000000000000, 1.000000000000000000 ) ) ;
#1567 = ADVANCED_FACE ( 'NONE', ( #8163 ), #7509, .T. ) ;
#1568 = CARTESIAN_POINT ( 'NONE',  ( 2.108492589042352705, -0.7506590739006395729, -2.134148098076933397 ) ) ;
#1569 = DIRECTION ( 'NONE',  ( 0.8660254037844402619, 0.4999999999999970579, -0.000000000000000000 ) ) ;
#1570 = CARTESIAN_POINT ( 'NONE',  ( 3.992485675378533383, -0.9493409260993608267, 1.674995433905599462 ) ) ;
#1571 = CARTESIAN_POINT ( 'NONE',  ( 2.625000000000002220, -27.35416666598386826, 4.546633369868302132 ) ) ;
#1572 = CARTESIAN_POINT ( 'NONE',  ( -5.250000000000000000, -27.68749999931720396, 0.000000000000000000 ) ) ;
#1573 = CARTESIAN_POINT ( 'NONE',  ( -2.624999999999998668, -26.94791666734946389, -4.546633369868303021 ) ) ;
#1574 = CARTESIAN_POINT ( 'NONE',  ( -6.420198811813273403E-16, -30.00000000000000000, 5.242490174541154069 ) ) ;
#1575 = EDGE_CURVE ( 'NONE', #803, #8842, #8724, .T. ) ;
#1576 = ORIENTED_EDGE ( 'NONE', *, *, #1464, .F. ) ;
#1577 = DIRECTION ( 'NONE',  ( 1.000000000000000000, 0.000000000000000000, 0.000000000000000000 ) ) ;
#1578 = CARTESIAN_POINT ( 'NONE',  ( 2.692658234375002735, -27.99479166632526628, 4.663820869356205101 ) ) ;
#1579 = DIRECTION ( 'NONE',  ( 0.000000000000000000, 0.000000000000000000, 1.000000000000000000 ) ) ;
#1580 = ORIENTED_EDGE ( 'NONE', *, *, #3015, .F. ) ;
#1581 = CARTESIAN_POINT ( 'NONE',  ( -5.114683531250001636, -26.96354166700806232, 2.952963913586931444 ) ) ;
#1582 = CARTESIAN_POINT ( 'NONE',  ( -1.224499502706140497, -3.250659073900639573, 3.007514324621436863 ) ) ;
#1583 = ORIENTED_EDGE ( 'NONE', *, *, #2917, .T. ) ;
#1584 = CARTESIAN_POINT ( 'NONE',  ( -5.250000000000000000, -28.87499999999999645, -6.429395695523604153E-16 ) ) ;
#1585 = CARTESIAN_POINT ( 'NONE',  ( -5.114683531250001636, -28.27604166700806587, 2.952963913586931444 ) ) ;
#1586 = EDGE_CURVE ( 'NONE', #7256, #3429, #6249, .T. ) ;
#1587 = CARTESIAN_POINT ( 'NONE',  ( 1.113604000661152470E-15, -27.68750000000000000, 6.062177826491070398 ) ) ;
#1588 = CARTESIAN_POINT ( 'NONE',  ( 5.114683531250000748, -29.85937500034139802, 0.000000000000000000 ) ) ;
#1589 = CARTESIAN_POINT ( 'NONE',  ( -3.492485675378536047, -6.549340926099363358, -1.467888652719048670 ) ) ;
#1590 = CARTESIAN_POINT ( 'NONE',  ( 1.000000000000000000, -35.00000000000000000, -1.118033988749894680 ) ) ;
#1591 = DIRECTION ( 'NONE',  ( 8.542704229054961664E-18, -0.9975640502598241977, 0.06975647374412545509 ) ) ;
#1592 = LINE ( 'NONE', #843, #2738 ) ;
#1593 = CYLINDRICAL_SURFACE ( 'NONE', #5686, 5.250000000000000000 ) ;
#1594 = ORIENTED_EDGE ( 'NONE', *, *, #3658, .F. ) ;
#1595 = CARTESIAN_POINT ( 'NONE',  ( 1.406733260263395735, -28.11383544963257464, 5.250000000000000000 ) ) ;
#1596 = CARTESIAN_POINT ( 'NONE',  ( -1.406733260263393293, -29.42633545031537423, -5.250000000000000000 ) ) ;
#1597 = CARTESIAN_POINT ( 'NONE',  ( -2.557341765625002594, -28.94270833367473017, 4.429445870380399164 ) ) ;
#1598 = VERTEX_POINT ( 'NONE', #7542 ) ;
#1599 = CARTESIAN_POINT ( 'NONE',  ( -1.406733260263402174, -29.69866454968462222, 5.249999999999995559 ) ) ;
#1600 = CARTESIAN_POINT ( 'NONE',  ( 5.385316468750001029, -27.75520833299194123, 3.109213912904134958 ) ) ;
#1601 = CARTESIAN_POINT ( 'NONE',  ( 3.992485675378568910, -3.850659073900639662, -1.674995433905514863 ) ) ;
#1602 = CARTESIAN_POINT ( 'NONE',  ( 5.250000000000000000, -27.50000000000000000, 0.000000000000000000 ) ) ;
#1603 = ORIENTED_EDGE ( 'NONE', *, *, #5041, .F. ) ;
#1604 = PRODUCT_DEFINITION_FORMATION_WITH_SPECIFIED_SOURCE ( 'ANY', '', #7829, .NOT_KNOWN. ) ;
#1605 = CARTESIAN_POINT ( 'NONE',  ( -1.975475456537005874E-15, -29.81249999999999645, 5.250000000000000000 ) ) ;
#1606 = DIRECTION ( 'NONE',  ( 0.000000000000000000, 1.000000000000000000, 0.000000000000000000 ) ) ;
#1607 = EDGE_CURVE ( 'NONE', #183, #2600, #6516, .T. ) ;
#1608 = CARTESIAN_POINT ( 'NONE',  ( 5.385316468750000141, -27.48437499965860198, -6.595110575850215044E-16 ) ) ;
#1609 = CARTESIAN_POINT ( 'NONE',  ( -5.114683531249999859, -29.81770833367473017, -2.952963913586935440 ) ) ;
#1610 = CARTESIAN_POINT ( 'NONE',  ( 1.406733260263405061, -27.47991455036742181, -5.249999999999994671 ) ) ;
#1611 = VECTOR ( 'NONE', #1569, 1000.000000000000114 ) ;
#1612 = CARTESIAN_POINT ( 'NONE',  ( 5.385316468750001029, -27.47395833299193413, 3.109213912904134958 ) ) ;
#1613 = CARTESIAN_POINT ( 'NONE',  ( 1.260781871532430598, -5.050659073900640728, 2.992485675378564469 ) ) ;
#1614 = UNCERTAINTY_MEASURE_WITH_UNIT (LENGTH_MEASURE( 1.000000000000000082E-05 ), #8120, 'distance_accuracy_value', 'NONE');
#1615 = FACE_OUTER_BOUND ( 'NONE', #3876, .T. ) ;
#1616 = CARTESIAN_POINT ( 'NONE',  ( 2.841254879263473310, -6.750659073900638241, 2.815599370228907272 ) ) ;
#1617 = EDGE_CURVE ( 'NONE', #6175, #7159, #6471, .T. ) ;
#1618 = CARTESIAN_POINT ( 'NONE',  ( 1.113604000661152470E-15, -27.87499999931720751, 6.062177826491070398 ) ) ;
#1619 = CARTESIAN_POINT ( 'NONE',  ( -1.406733260263394625, -27.73883544963256753, -5.250000000000000000 ) ) ;
#1620 = AXIS2_PLACEMENT_3D ( 'NONE', #2317, #4453, #5145 ) ;
#1621 = CARTESIAN_POINT ( 'NONE',  ( 1.467888652719048226, -1.349340926099361182, -3.492485675378535603 ) ) ;
#1622 = CARTESIAN_POINT ( 'NONE',  ( 5.250000000000000000, -29.06249999931720396, -6.429395695523604153E-16 ) ) ;
#1623 = ORIENTED_EDGE ( 'NONE', *, *, #8749, .F. ) ;
#1624 = CARTESIAN_POINT ( 'NONE',  ( -5.385316468750001029, -28.84895833299193413, -3.109213912904136734 ) ) ;
#1625 = CARTESIAN_POINT ( 'NONE',  ( 4.007514324621469726, -2.749340926099360427, -1.638713065079161257 ) ) ;
#1626 = FACE_OUTER_BOUND ( 'NONE', #4285, .T. ) ;
#1627 = EDGE_LOOP ( 'NONE', ( #6721, #320, #992, #4948 ) ) ;
#1628 = AXIS2_PLACEMENT_3D ( 'NONE', #5867, #799, #3688 ) ;
#1629 = CARTESIAN_POINT ( 'NONE',  ( 5.114683531249998971, -26.88020833367473017, 2.952963913586936329 ) ) ;
#1630 = CARTESIAN_POINT ( 'NONE',  ( 1.467888652718972731, -0.2506590739006389068, 3.492485675378566246 ) ) ;
#1631 = ORIENTED_EDGE ( 'NONE', *, *, #8037, .F. ) ;
#1632 = CARTESIAN_POINT ( 'NONE',  ( -5.250000000000000000, -28.14583333333333215, -3.031088913245536531 ) ) ;
#1633 = VECTOR ( 'NONE', #3430, 1000.000000000000114 ) ;
#1634 = CARTESIAN_POINT ( 'NONE',  ( 3.616337804771879580E-16, -28.10937500034139802, -5.905927827173866440 ) ) ;
#1635 = AXIS2_PLACEMENT_3D ( 'NONE', #8434, #6111, #4845 ) ;
#1636 = CARTESIAN_POINT ( 'NONE',  ( 2.624999999999998668, -27.33333333333333570, -4.546633369868303021 ) ) ;
#1637 = AXIS2_PLACEMENT_3D ( 'NONE', #1137, #4623, #5581 ) ;
#1638 = CARTESIAN_POINT ( 'NONE',  ( 0.000000000000000000, -29.00000000000000355, 0.000000000000000000 ) ) ;
#1639 =( BOUNDED_SURFACE ( )  B_SPLINE_SURFACE ( 1, 2, ( 
 ( #3225, #7455, #889, #1081, #6750, #5302, #4427, #938, #3182, #6047, #7312, #7962, #8884, #7404, #5258, #3827, #1636, #5114, #5165, #1028, #8056, #6609, #6003, #238, #3088, #8753, #3877, #3138, #2383, #1685, #4526, #6652, #8841, #1587, #5959, #7262, #7356, #2433, #1732, #611, #6797, #2671, #5495, #6240, #3366, #1882, #6151, #1129, #4061, #8386, #5540, #2013, #6197, #9025, #8930, #3452, #474, #2578, #6281, #1267, #1924, #7501, #4838, #2715, #567, #422, #7640, #524, #4106, #6900, #3319, #4016, #8341, #8979, #6938, #1828, #8199, #2628, #4662, #1968, #4796, #7683, #4752, #3411, #9072, #1306, #5446, #3969, #7596, #4148, #5350, #1221, #6984, #2526, #3270, #8292, #6099, #5398, #8249, #4707, #7546, #1172, #6850, #3584, #4282, #8599, #2099, #5670, #737, #4374, #5713, #4239, #4965, #3496, #655, #694, #8518, #6453, #7026, #4923, #3676, #6363, #7775, #7730, #3539, #9118, #5758, #1397, #831, #6320, #2055, #7069, #87, #5624, #8556, #5005, #2763, #1483, #2805, #2184, #7862, #3, #8427, #7909, #2853 ),
 ( #2144, #5583, #2231, #8475, #7206, #5056, #4880, #1530, #1354, #2937, #4193, #7819, #4327, #9156, #1435, #7113, #6408, #7160, #46, #2895, #786, #3631, #5105, #5948, #6599, #4419, #8092, #7953, #5854, #7250, #8787, #4515, #3034, #180, #3773, #5202, #5248, #2418, #2373, #6498, #876, #229, #1769, #4604, #1578, #6642, #271, #1016, #7345, #8694, #923, #3726, #8044, #3170, #317, #5992, #970, #3817, #6549, #7443, #4463, #2324, #1068, #1721, #5899, #2279, #8831, #6687, #4557, #5153, #7393, #3124, #3864, #1672, #7301, #7997, #2467, #3078, #5291, #5809, #2984, #8739, #8647, #8141, #133, #1624, #6136, #9014, #7629, #8329, #4694, #2512, #8967, #6930, #6734, #2617, #4096, #4786, #6034, #1160, #6230, #2003, #6885, #5339, #3356, #8872, #3214, #2703, #7532, #558, #512, #1258, #6186, #2659, #4051, #4738, #1871, #9062, #5481, #1960, #4829, #3402, #410, #6838, #5532, #8188, #4004, #1817, #5434, #8376, #7674, #8280, #2567, #4649, #462, #3910, #365, #7490, #1116, #3957, #6784, #5386, #1913, #3306, #7585 ) ),
 .UNSPECIFIED., .F., .F., .F. ) 
 B_SPLINE_SURFACE_WITH_KNOTS ( ( 2, 2 ),
 ( 3, 2, 2, 2, 2, 2, 2, 2, 2, 2, 2, 2, 2, 2, 2, 2, 2, 2, 2, 2, 2, 2, 2, 2, 2, 2, 2, 2, 2, 2, 2, 2, 2, 2, 2, 2, 2, 2, 2, 2, 2, 2, 2, 2, 2, 2, 2, 2, 2, 2, 2, 2, 2, 2, 2, 2, 2, 2, 2, 2, 2, 2, 2, 2, 2, 2, 2, 2, 2, 2, 2, 2, 3 ),
 ( 0.000000000000000000, 1.000000000000000000 ),
 ( 0.000000000000000000, 0.01388888888888888812, 0.02777777777777777624, 0.04166666666666666435, 0.05555555555555555247, 0.06944444444444444753, 0.08333333333333332871, 0.09722222222222222376, 0.1111111111111111049, 0.1250000000000000000, 0.1388888888888888951, 0.1527777777777777901, 0.1666666666666666574, 0.1805555555555555525, 0.1944444444444444475, 0.2083333333333333426, 0.2222222222222222099, 0.2361111111111111049, 0.2500000000000000000, 0.2638888888888888951, 0.2777777777777777901, 0.2916666666666666852, 0.3055555555555555802, 0.3194444444444444198, 0.3333333333333333148, 0.3472222222222222099, 0.3611111111111111049, 0.3750000000000000000, 0.3888888888888888951, 0.4027777777777777901, 0.4166666666666666852, 0.4305555555555555802, 0.4444444444444444198, 0.4583333333333333148, 0.4722222222222222099, 0.4861111111111111049, 0.5000000000000000000, 0.5138888888888888395, 0.5277777777777777901, 0.5416666666666666297, 0.5555555555555555802, 0.5694444444444444198, 0.5833333333333333703, 0.5972222222222222099, 0.6111111111111111605, 0.6250000000000000000, 0.6388888888888888395, 0.6527777777777777901, 0.6666666666666666297, 0.6805555555555555802, 0.6944444444444444198, 0.7083333333333333703, 0.7222222222222222099, 0.7361111111111111605, 0.7500000000000000000, 0.7638888888888888395, 0.7777777777777777901, 0.7916666666666666297, 0.8055555555555555802, 0.8194444444444444198, 0.8333333333333333703, 0.8472222222222222099, 0.8611111111111111605, 0.8750000000000000000, 0.8888888888888888395, 0.9027777777777777901, 0.9166666666666666297, 0.9305555555555555802, 0.9444444444444444198, 0.9583333333333333703, 0.9722222222222222099, 0.9861111111111111605, 1.000000000000000000 ),
 .UNSPECIFIED. ) 
 GEOMETRIC_REPRESENTATION_ITEM ( )  RATIONAL_B_SPLINE_SURFACE ( (
 ( 1.000000000000000000, 0.8660254037844387076, 1.000000000000000000, 0.8660254037844387076, 1.000000000000000000, 0.8660254037844387076, 1.000000000000000000, 0.8660254037844387076, 1.000000000000000000, 0.8660254037844387076, 1.000000000000000000, 0.8660254037844387076, 1.000000000000000000, 0.8660254037844387076, 1.000000000000000000, 0.8660254037844387076, 1.000000000000000000, 0.8660254037844387076, 1.000000000000000000, 0.8660254037844387076, 1.000000000000000000, 0.8660254037844387076, 1.000000000000000000, 0.8660254037844387076, 1.000000000000000000, 0.8660254037844387076, 1.000000000000000000, 0.8660254037844387076, 1.000000000000000000, 0.8660254037844387076, 1.000000000000000000, 0.8660254037844387076, 1.000000000000000000, 0.8660254037844387076, 1.000000000000000000, 0.8660254037844387076, 1.000000000000000000, 0.8660254037844387076, 1.000000000000000000, 0.8660254037844387076, 1.000000000000000000, 0.8660254037844387076, 1.000000000000000000, 0.8660254037844387076, 1.000000000000000000, 0.8660254037844387076, 1.000000000000000000, 0.8660254037844387076, 1.000000000000000000, 0.8660254037844387076, 1.000000000000000000, 0.8660254037844387076, 1.000000000000000000, 0.8660254037844387076, 1.000000000000000000, 0.8660254037844387076, 1.000000000000000000, 0.8660254037844387076, 1.000000000000000000, 0.8660254037844387076, 1.000000000000000000, 0.8660254037844387076, 1.000000000000000000, 0.8660254037844387076, 1.000000000000000000, 0.8660254037844387076, 1.000000000000000000, 0.8660254037844387076, 1.000000000000000000, 0.8660254037844387076, 1.000000000000000000, 0.8660254037844387076, 1.000000000000000000, 0.8660254037844387076, 1.000000000000000000, 0.8660254037844387076, 1.000000000000000000, 0.8660254037844387076, 1.000000000000000000, 0.8660254037844387076, 1.000000000000000000, 0.8660254037844387076, 1.000000000000000000, 0.8660254037844387076, 1.000000000000000000, 0.8660254037844387076, 1.000000000000000000, 0.8660254037844387076, 1.000000000000000000, 0.8660254037844387076, 1.000000000000000000, 0.8660254037844387076, 1.000000000000000000, 0.8660254037844387076, 1.000000000000000000, 0.8660254037844387076, 1.000000000000000000, 0.8660254037844387076, 1.000000000000000000, 0.8660254037844387076, 1.000000000000000000, 0.8660254037844387076, 1.000000000000000000, 0.8660254037844387076, 1.000000000000000000, 0.8660254037844387076, 1.000000000000000000, 0.8660254037844387076, 1.000000000000000000, 0.8660254037844387076, 1.000000000000000000, 0.8660254037844387076, 1.000000000000000000, 0.8660254037844387076, 1.000000000000000000, 0.8660254037844387076, 1.000000000000000000, 0.8660254037844387076, 1.000000000000000000, 0.8660254037844387076, 1.000000000000000000, 0.8660254037844387076, 1.000000000000000000, 0.8660254037844387076, 1.000000000000000000, 0.8660254037844387076, 1.000000000000000000, 0.8660254037844387076, 1.000000000000000000, 0.8660254037844387076, 1.000000000000000000, 0.8660254037844387076, 1.000000000000000000, 0.8660254037844387076, 1.000000000000000000, 0.8660254037844387076, 1.000000000000000000, 0.8660254037844387076, 1.000000000000000000, 0.8660254037844387076, 1.000000000000000000, 0.8660254037844387076, 1.000000000000000000, 0.8660254037844387076, 1.000000000000000000),
 ( 1.000000000000000000, 0.8660254037844387076, 1.000000000000000000, 0.8660254037844387076, 1.000000000000000000, 0.8660254037844387076, 1.000000000000000000, 0.8660254037844387076, 1.000000000000000000, 0.8660254037844387076, 1.000000000000000000, 0.8660254037844387076, 1.000000000000000000, 0.8660254037844387076, 1.000000000000000000, 0.8660254037844387076, 1.000000000000000000, 0.8660254037844387076, 1.000000000000000000, 0.8660254037844387076, 1.000000000000000000, 0.8660254037844387076, 1.000000000000000000, 0.8660254037844387076, 1.000000000000000000, 0.8660254037844387076, 1.000000000000000000, 0.8660254037844387076, 1.000000000000000000, 0.8660254037844387076, 1.000000000000000000, 0.8660254037844387076, 1.000000000000000000, 0.8660254037844387076, 1.000000000000000000, 0.8660254037844387076, 1.000000000000000000, 0.8660254037844387076, 1.000000000000000000, 0.8660254037844387076, 1.000000000000000000, 0.8660254037844387076, 1.000000000000000000, 0.8660254037844387076, 1.000000000000000000, 0.8660254037844387076, 1.000000000000000000, 0.8660254037844387076, 1.000000000000000000, 0.8660254037844387076, 1.000000000000000000, 0.8660254037844387076, 1.000000000000000000, 0.8660254037844387076, 1.000000000000000000, 0.8660254037844387076, 1.000000000000000000, 0.8660254037844387076, 1.000000000000000000, 0.8660254037844387076, 1.000000000000000000, 0.8660254037844387076, 1.000000000000000000, 0.8660254037844387076, 1.000000000000000000, 0.8660254037844387076, 1.000000000000000000, 0.8660254037844387076, 1.000000000000000000, 0.8660254037844387076, 1.000000000000000000, 0.8660254037844387076, 1.000000000000000000, 0.8660254037844387076, 1.000000000000000000, 0.8660254037844387076, 1.000000000000000000, 0.8660254037844387076, 1.000000000000000000, 0.8660254037844387076, 1.000000000000000000, 0.8660254037844387076, 1.000000000000000000, 0.8660254037844387076, 1.000000000000000000, 0.8660254037844387076, 1.000000000000000000, 0.8660254037844387076, 1.000000000000000000, 0.8660254037844387076, 1.000000000000000000, 0.8660254037844387076, 1.000000000000000000, 0.8660254037844387076, 1.000000000000000000, 0.8660254037844387076, 1.000000000000000000, 0.8660254037844387076, 1.000000000000000000, 0.8660254037844387076, 1.000000000000000000, 0.8660254037844387076, 1.000000000000000000, 0.8660254037844387076, 1.000000000000000000, 0.8660254037844387076, 1.000000000000000000, 0.8660254037844387076, 1.000000000000000000, 0.8660254037844387076, 1.000000000000000000, 0.8660254037844387076, 1.000000000000000000, 0.8660254037844387076, 1.000000000000000000, 0.8660254037844387076, 1.000000000000000000, 0.8660254037844387076, 1.000000000000000000, 0.8660254037844387076, 1.000000000000000000, 0.8660254037844387076, 1.000000000000000000, 0.8660254037844387076, 1.000000000000000000, 0.8660254037844387076, 1.000000000000000000, 0.8660254037844387076, 1.000000000000000000, 0.8660254037844387076, 1.000000000000000000, 0.8660254037844387076, 1.000000000000000000, 0.8660254037844387076, 1.000000000000000000, 0.8660254037844387076, 1.000000000000000000, 0.8660254037844387076, 1.000000000000000000, 0.8660254037844387076, 1.000000000000000000, 0.8660254037844387076, 1.000000000000000000, 0.8660254037844387076, 1.000000000000000000) ) ) 
 REPRESENTATION_ITEM ( '' )  SURFACE ( )  );
#1640 = CARTESIAN_POINT ( 'NONE',  ( 3.492485675378536047, -0.9493409260993610488, 1.467888652719046672 ) ) ;
#1641 = DIRECTION ( 'NONE',  ( 0.000000000000000000, 0.000000000000000000, 1.000000000000000000 ) ) ;
#1642 = CARTESIAN_POINT ( 'NONE',  ( 5.249999999999997335, -28.77083333333333215, 3.031088913245538308 ) ) ;
#1643 = CARTESIAN_POINT ( 'NONE',  ( 5.114683531249998971, -28.44270833367473017, 2.952963913586936329 ) ) ;
#1644 = FACE_OUTER_BOUND ( 'NONE', #1282, .T. ) ;
#1645 = EDGE_CURVE ( 'NONE', #2851, #105, #3332, .T. ) ;
#1646 = ORIENTED_EDGE ( 'NONE', *, *, #5983, .T. ) ;
#1647 = CARTESIAN_POINT ( 'NONE',  ( -5.249999999999999112, -28.67708333401612464, -3.031088913245536975 ) ) ;
#1648 = CARTESIAN_POINT ( 'NONE',  ( 5.249999999999997335, -27.05208333401612819, 3.031088913245538308 ) ) ;
#1649 = AXIS2_PLACEMENT_3D ( 'NONE', #4104, #3450, #8927 ) ;
#1650 = CARTESIAN_POINT ( 'NONE',  ( 5.114683531249998971, -28.63020833367472662, 2.952963913586936329 ) ) ;
#1651 = ORIENTED_EDGE ( 'NONE', *, *, #2549, .T. ) ;
#1652 = CARTESIAN_POINT ( 'NONE',  ( -5.385316468750000141, -27.09374999965859843, 0.000000000000000000 ) ) ;
#1653 = CARTESIAN_POINT ( 'NONE',  ( 5.385316468749999252, -27.96354166632526628, -3.109213912904138954 ) ) ;
#1654 = CARTESIAN_POINT ( 'NONE',  ( -2.815599370228907272, -4.750659073900638241, 2.841254879263473754 ) ) ;
#1655 = CARTESIAN_POINT ( 'NONE',  ( 1.406733260263391960, -27.55133545031536713, 5.250000000000000000 ) ) ;
#1656 = EDGE_LOOP ( 'NONE', ( #1731, #692, #8798, #2540 ) ) ;
#1657 = DIRECTION ( 'NONE',  ( 0.000000000000000000, -0.000000000000000000, -1.000000000000000000 ) ) ;
#1658 = CARTESIAN_POINT ( 'NONE',  ( -1.113604000661152470E-15, -28.84375000068279959, 6.062177826491070398 ) ) ;
#1659 = EDGE_CURVE ( 'NONE', #3226, #1074, #5924, .T. ) ;
#1660 = CARTESIAN_POINT ( 'NONE',  ( -2.692658234375000514, -27.65104166632526628, -4.663820869356205989 ) ) ;
#1661 = CARTESIAN_POINT ( 'NONE',  ( -1.084901341431563923E-15, -27.67187500034140157, 5.905927827173866440 ) ) ;
#1662 = ORIENTED_EDGE ( 'NONE', *, *, #4479, .F. ) ;
#1663 = CARTESIAN_POINT ( 'NONE',  ( 5.385316468750000141, -27.45312499965860198, -6.595110575850215044E-16 ) ) ;
#1664 = CARTESIAN_POINT ( 'NONE',  ( -3.007514324621435531, -4.450659073900640195, -1.224499502706142273 ) ) ;
#1665 = CARTESIAN_POINT ( 'NONE',  ( -1.406733260263393070, -27.48883544963257108, -5.250000000000000888 ) ) ;
#1666 = CARTESIAN_POINT ( 'NONE',  ( -3.992485675378532939, -3.349340926099360960, -1.674995433905601683 ) ) ;
#1667 = CARTESIAN_POINT ( 'NONE',  ( -3.712013335537174572E-16, -27.74999999931720396, -6.062177826491070398 ) ) ;
#1668 = CARTESIAN_POINT ( 'NONE',  ( -1.406733260263394625, -27.05133545031536713, -5.250000000000000000 ) ) ;
#1669 = CARTESIAN_POINT ( 'NONE',  ( 3.507514324621465285, -5.949340926099361049, -1.431606283892619347 ) ) ;
#1670 = CARTESIAN_POINT ( 'NONE',  ( 1.406733260263385521, -29.86383544963257108, 5.250000000000006217 ) ) ;
#1671 = EDGE_CURVE ( 'NONE', #2249, #5349, #3580, .T. ) ;
#1672 = CARTESIAN_POINT ( 'NONE',  ( -5.385316468750001029, -28.59895833299193413, -3.109213912904136734 ) ) ;
#1673 = CARTESIAN_POINT ( 'NONE',  ( -4.000000000000000000, -5.049340926099361582, -0.01814118441321865144 ) ) ;
#1674 = DIRECTION ( 'NONE',  ( 0.000000000000000000, -1.000000000000000000, 0.000000000000000000 ) ) ;
#1675 = ORIENTED_EDGE ( 'NONE', *, *, #4460, .T. ) ;
#1676 = CARTESIAN_POINT ( 'NONE',  ( -2.692658234374996518, -27.78645833299193413, 4.663820869356208654 ) ) ;
#1677 = CARTESIAN_POINT ( 'NONE',  ( -0.01814118441313947866, -0.9506590739006390844, -3.500000000000000000 ) ) ;
#1678 = CIRCLE ( 'NONE', #5541, 2.750000000000000000 ) ;
#1679 = ORIENTED_EDGE ( 'NONE', *, *, #313, .T. ) ;
#1680 = CARTESIAN_POINT ( 'NONE',  ( 3.712013335537174572E-16, -27.68750000000000000, -6.062177826491070398 ) ) ;
#1681 = CARTESIAN_POINT ( 'NONE',  ( -2.557341765624999042, -28.33854166700806587, -4.429445870380400052 ) ) ;
#1682 = CIRCLE ( 'NONE', #6140, 6.250000000000000000 ) ;
#1683 = AXIS2_PLACEMENT_3D ( 'NONE', #7363, #987, #4483 ) ;
#1684 =( NAMED_UNIT ( * ) PLANE_ANGLE_UNIT ( ) SI_UNIT ( $, .RADIAN. ) );
#1685 = CARTESIAN_POINT ( 'NONE',  ( 5.250000000000000000, -27.60416666666666785, -3.031088913245536531 ) ) ;
#1686 = ADVANCED_FACE ( 'NONE', ( #7882 ), #5347, .T. ) ;
#1687 = CARTESIAN_POINT ( 'NONE',  ( 2.624999999999998668, -30.02083333265053611, -4.546633369868303021 ) ) ;
#1688 = CARTESIAN_POINT ( 'NONE',  ( 2.487701488670255756, -4.449340926099361937, -2.462045979635577364 ) ) ;
#1689 = CARTESIAN_POINT ( 'NONE',  ( 0.000000000000000000, -53.00000000000000000, 2.549999999999999822 ) ) ;
#1690 = CARTESIAN_POINT ( 'NONE',  ( 2.624999999999996891, -28.79166666666666785, 4.546633369868304797 ) ) ;
#1691 = CARTESIAN_POINT ( 'NONE',  ( -2.557341765625002594, -29.25520833367473017, 4.429445870380399164 ) ) ;
#1692 = CARTESIAN_POINT ( 'NONE',  ( 5.249999999999999112, -28.26041666734946745, -3.031088913245534755 ) ) ;
#1693 = CIRCLE ( 'NONE', #8384, 5.250000000000000000 ) ;
#1694 = ORIENTED_EDGE ( 'NONE', *, *, #6925, .F. ) ;
#1695 = DIRECTION ( 'NONE',  ( 1.000000000000000000, 0.000000000000000000, 0.000000000000000000 ) ) ;
#1696 = CARTESIAN_POINT ( 'NONE',  ( 5.114683531249999859, -28.08854166700806232, -2.952963913586932776 ) ) ;
#1697 = SHAPE_REPRESENTATION ( 'spring', ( #888 ), #3388 ) ;
#1698 = ORIENTED_EDGE ( 'NONE', *, *, #8246, .F. ) ;
#1699 = CYLINDRICAL_SURFACE ( 'NONE', #1849, 5.250000000000000000 ) ;
#1700 = CARTESIAN_POINT ( 'NONE',  ( -3.807688866302469071E-16, -27.42187499965860198, -6.218427825808274356 ) ) ;
#1701 = CARTESIAN_POINT ( 'NONE',  ( 3.992485675378568910, -7.050659073900638063, -1.674995433905514863 ) ) ;
#1702 = CARTESIAN_POINT ( 'NONE',  ( -2.624999999999998668, -29.16666666666666785, -4.546633369868303021 ) ) ;
#1703 = CARTESIAN_POINT ( 'NONE',  ( 5.385316468749999252, -27.96354166632526628, -3.109213912904139399 ) ) ;
#1704 = VERTEX_POINT ( 'NONE', #7451 ) ;
#1705 = FACE_OUTER_BOUND ( 'NONE', #3131, .T. ) ;
#1706 = CARTESIAN_POINT ( 'NONE',  ( 2.625000000000000444, -28.73958333401612819, -4.546633369868303021 ) ) ;
#1707 = CARTESIAN_POINT ( 'NONE',  ( -2.692658234374996518, -28.31770833299193413, 4.663820869356208654 ) ) ;
#1708 = CARTESIAN_POINT ( 'NONE',  ( -2.557341765624999042, -27.77604166700806587, -4.429445870380400052 ) ) ;
#1709 = ORIENTED_EDGE ( 'NONE', *, *, #5661, .T. ) ;
#1710 = FACE_OUTER_BOUND ( 'NONE', #3361, .T. ) ;
#1711 = CARTESIAN_POINT ( 'NONE',  ( 1.260781871532430598, -3.450659073900639751, 2.992485675378564469 ) ) ;
#1712 = CARTESIAN_POINT ( 'NONE',  ( -5.250000000000000000, -27.43749999931720396, 0.000000000000000000 ) ) ;
#1713 = CARTESIAN_POINT ( 'NONE',  ( 5.250000000000000000, -27.81249999931720396, -6.429395695523604153E-16 ) ) ;
#1714 = DIRECTION ( 'NONE',  ( 0.000000000000000000, -1.000000000000000000, 0.000000000000000000 ) ) ;
#1715 = CARTESIAN_POINT ( 'NONE',  ( 0.01814118441321408565, -3.049340926099361138, -3.500000000000000000 ) ) ;
#1716 = PRODUCT_RELATED_PRODUCT_CATEGORY ( 'part', '', ( #3523 ) ) ;
#1717 = FACE_OUTER_BOUND ( 'NONE', #1005, .T. ) ;
#1718 = DIRECTION ( 'NONE',  ( 0.000000000000000000, -1.000000000000000000, 0.000000000000000000 ) ) ;
#1719 = PRESENTATION_STYLE_ASSIGNMENT (( #969 ) ) ;
#1720 =( BOUNDED_CURVE ( )  B_SPLINE_CURVE ( 2, ( #8620, #898, #947, #1648, #3748, #8576, #7222, #8668, #3835 ),
 .UNSPECIFIED., .F., .T. ) 
 B_SPLINE_CURVE_WITH_KNOTS ( ( 3, 2, 2, 2, 3 ),
 ( 0.8958333333333333703, 0.9027777777777777901, 0.9166666666666666297, 0.9305555555555555802, 0.9375000000000000000 ),
 .UNSPECIFIED. ) 
 CURVE ( )  GEOMETRIC_REPRESENTATION_ITEM ( )  RATIONAL_B_SPLINE_CURVE ( ( 0.9330127018922192983, 0.9330127018922198534, 1.000000000000000000, 0.8660254037844387076, 1.000000000000000000, 0.8660254037844387076, 1.000000000000000000, 0.9330127018922194093, 0.9330127018922194093 ) ) 
 REPRESENTATION_ITEM ( '' )  );
#1721 = CARTESIAN_POINT ( 'NONE',  ( -3.807688866302469071E-16, -28.39062499965859843, -6.218427825808274356 ) ) ;
#1722 = CARTESIAN_POINT ( 'NONE',  ( 3.992485675378533383, -5.749340926099361759, 1.674995433905599462 ) ) ;
#1723 = CARTESIAN_POINT ( 'NONE',  ( -1.406733260263382856, -27.42633545031536713, -5.250000000000006217 ) ) ;
#1724 = VERTEX_POINT ( 'NONE', #8575 ) ;
#1725 = CARTESIAN_POINT ( 'NONE',  ( 2.692658234375002735, -27.74479166632526628, 4.663820869356205101 ) ) ;
#1726 = CARTESIAN_POINT ( 'NONE',  ( -0.01814118441314477650, -5.750659073900639129, -3.000000000000000444 ) ) ;
#1727 = ORIENTED_EDGE ( 'NONE', *, *, #6142, .F. ) ;
#1728 = CARTESIAN_POINT ( 'NONE',  ( 2.625000000000000444, -27.70833333333333215, -4.546633369868303021 ) ) ;
#1729 = CARTESIAN_POINT ( 'NONE',  ( 3.500000000000000000, -2.150659073900639040, -0.01814118441313969030 ) ) ;
#1730 = EDGE_CURVE ( 'NONE', #813, #2168, #7834, .T. ) ;
#1731 = ORIENTED_EDGE ( 'NONE', *, *, #222, .F. ) ;
#1732 = CARTESIAN_POINT ( 'NONE',  ( -2.625000000000000444, -27.79166666666666430, -4.546633369868303021 ) ) ;
#1733 = ORIENTED_EDGE ( 'NONE', *, *, #2223, .T. ) ;
#1734 = CARTESIAN_POINT ( 'NONE',  ( -2.557341765625002594, -28.44270833367473017, 4.429445870380399164 ) ) ;
#1735 = EDGE_CURVE ( 'NONE', #3199, #5007, #9069, .T. ) ;
#1736 = CARTESIAN_POINT ( 'NONE',  ( 1.431606283892619125, -2.349340926099361848, 3.507514324621464397 ) ) ;
#1737 = CARTESIAN_POINT ( 'NONE',  ( 2.161402558328724325E-14, -29.49999999931720396, -5.250000000000000000 ) ) ;
#1738 = CARTESIAN_POINT ( 'NONE',  ( 0.000000000000000000, -30.00000000000000000, 5.250000000000000000 ) ) ;
#1739 = CARTESIAN_POINT ( 'NONE',  ( -5.114683531250000748, -28.79687500034139802, -6.263680815196995234E-16 ) ) ;
#1740 = CARTESIAN_POINT ( 'NONE',  ( 2.300847884672513123E-14, -28.21875000068279604, -5.250000000000000000 ) ) ;
#1741 = ORIENTED_EDGE ( 'NONE', *, *, #768, .F. ) ;
#1742 = CARTESIAN_POINT ( 'NONE',  ( 6.972266317189433020E-16, -29.93749999999999645, -5.249999999999999112 ) ) ;
#1743 = CARTESIAN_POINT ( 'NONE',  ( -5.114683531249999859, -27.75520833367473017, -2.952963913586935440 ) ) ;
#1744 = ORIENTED_EDGE ( 'NONE', *, *, #3503, .T. ) ;
#1745 =( GEOMETRIC_REPRESENTATION_CONTEXT ( 3 ) GLOBAL_UNCERTAINTY_ASSIGNED_CONTEXT ( ( #5793 ) ) GLOBAL_UNIT_ASSIGNED_CONTEXT ( ( #3922, #7355, #8883 ) ) REPRESENTATION_CONTEXT ( 'NONE', 'WORKASPACE' ) );
#1746 = CARTESIAN_POINT ( 'NONE',  ( 0.000000000000000000, 70.00000000000000000, 0.000000000000000000 ) ) ;
#1747 = CARTESIAN_POINT ( 'NONE',  ( -5.385316468750000141, -28.85937499965860198, 0.000000000000000000 ) ) ;
#1748 = CARTESIAN_POINT ( 'NONE',  ( -2.841254879263473310, -7.550659073900639839, -2.815599370228907716 ) ) ;
#1749 = UNCERTAINTY_MEASURE_WITH_UNIT (LENGTH_MEASURE( 1.000000000000000082E-05 ), #4938, 'distance_accuracy_value', 'NONE');
#1750 = DIRECTION ( 'NONE',  ( 0.000000000000000000, 0.000000000000000000, 1.000000000000000000 ) ) ;
#1751 = CARTESIAN_POINT ( 'NONE',  ( -5.385316468749998364, -27.83854166632526628, 3.109213912904140287 ) ) ;
#1752 = VERTEX_POINT ( 'NONE', #7681 ) ;
#1753 = CARTESIAN_POINT ( 'NONE',  ( -1.406733260263395735, -29.82366454968462932, 5.250000000000000000 ) ) ;
#1754 = CARTESIAN_POINT ( 'NONE',  ( -5.250000000000000000, -27.90625000068279604, -6.429395695523604153E-16 ) ) ;
#1755 = PRODUCT_DEFINITION_FORMATION_WITH_SPECIFIED_SOURCE ( 'ANY', '', #4597, .NOT_KNOWN. ) ;
#1756 = CARTESIAN_POINT ( 'NONE',  ( -3.807688866302469071E-16, -27.67187499965859843, -6.218427825808274356 ) ) ;
#1757 = ORIENTED_EDGE ( 'NONE', *, *, #2513, .F. ) ;
#1758 = CARTESIAN_POINT ( 'NONE',  ( 1.142306659890740623E-15, -28.76562499965860553, 6.218427825808274356 ) ) ;
#1759 = CARTESIAN_POINT ( 'NONE',  ( 2.134148098076933397, -5.150659073900639484, 2.108492589042352261 ) ) ;
#1760 = CARTESIAN_POINT ( 'NONE',  ( 0.000000000000000000, -20.00000000000000000, 0.000000000000000000 ) ) ;
#1761 = ADVANCED_FACE ( 'NONE', ( #3408 ), #608, .T. ) ;
#1762 = EDGE_CURVE ( 'NONE', #7067, #8842, #6237, .T. ) ;
#1763 = CARTESIAN_POINT ( 'NONE',  ( -3.712013335537174572E-16, -27.99999999931720396, -6.062177826491070398 ) ) ;
#1764 = CARTESIAN_POINT ( 'NONE',  ( -5.250000000000000000, -27.00000000000000000, 0.000000000000000000 ) ) ;
#1765 = CARTESIAN_POINT ( 'NONE',  ( 0.01814118441321408565, -4.649340926099361226, -3.500000000000000000 ) ) ;
#1766 = CIRCLE ( 'NONE', #719, 2.500000000000000444 ) ;
#1767 = CARTESIAN_POINT ( 'NONE',  ( 5.114683531249998971, -29.63020833367473017, 2.952963913586936329 ) ) ;
#1768 = ORIENTED_EDGE ( 'NONE', *, *, #2025, .T. ) ;
#1769 = CARTESIAN_POINT ( 'NONE',  ( 5.385316468750000141, -27.95312499965860198, -6.595110575850215044E-16 ) ) ;
#1770 = CARTESIAN_POINT ( 'NONE',  ( 1.674995433905601239, -7.749340926099362648, -3.992485675378532939 ) ) ;
#1771 = CARTESIAN_POINT ( 'NONE',  ( 1.836970198721030181E-16, -20.00000000000000000, 1.500000000000000222 ) ) ;
#1772 = EDGE_LOOP ( 'NONE', ( #1220, #9002, #6481, #6040 ) ) ;
#1773 = CARTESIAN_POINT ( 'NONE',  ( 5.385316468750001029, -28.22395833299193058, 3.109213912904135846 ) ) ;
#1774 = CARTESIAN_POINT ( 'NONE',  ( -2.487701488670202910, -4.350659073900638774, -2.462045979635629767 ) ) ;
#1775 = ORIENTED_EDGE ( 'NONE', *, *, #2638, .T. ) ;
#1776 = CARTESIAN_POINT ( 'NONE',  ( 3.712013335537174572E-16, -28.43750000000000000, -6.062177826491070398 ) ) ;
#1777 = AXIS2_PLACEMENT_3D ( 'NONE', #4129, #3393, #7622 ) ;
#1778 = CARTESIAN_POINT ( 'NONE',  ( -3.492485675378566246, -3.050659073900638951, 1.467888652718973175 ) ) ;
#1779 =( BOUNDED_CURVE ( )  B_SPLINE_CURVE ( 2, ( #4094, #556, #3399, #6228, #2884, #4315, #1426, #1610, #4449 ),
 .UNSPECIFIED., .F., .F. ) 
 B_SPLINE_CURVE_WITH_KNOTS ( ( 3, 2, 2, 2, 3 ),
 ( 0.7291666666666667407, 0.7361111111111111605, 0.7500000000000000000, 0.7638888888888888395, 0.7708333333333332593 ),
 .UNSPECIFIED. ) 
 CURVE ( )  GEOMETRIC_REPRESENTATION_ITEM ( )  RATIONAL_B_SPLINE_CURVE ( ( 0.9330127018922192983, 0.9330127018922198534, 1.000000000000000000, 0.8660254037844387076, 1.000000000000000000, 0.8660254037844387076, 1.000000000000000000, 0.9330127018922198534, 0.9330127018922192983 ) ) 
 REPRESENTATION_ITEM ( '' )  );
#1780 = ORIENTED_EDGE ( 'NONE', *, *, #4907, .F. ) ;
#1781 =( LENGTH_UNIT ( ) NAMED_UNIT ( * ) SI_UNIT ( .MILLI., .METRE. ) );
#1782 = AXIS2_PLACEMENT_3D ( 'NONE', #3671, #1527, #4513 ) ;
#1783 = EDGE_LOOP ( 'NONE', ( #3498, #8024, #3217, #7823 ) ) ;
#1784 = CARTESIAN_POINT ( 'NONE',  ( -1.084901341431563726E-15, -29.42187500034139447, 5.905927827173866440 ) ) ;
#1785 = CARTESIAN_POINT ( 'NONE',  ( -1.260781871532494103, -3.749340926099361315, 2.992485675378538712 ) ) ;
#1786 = VECTOR ( 'NONE', #5974, 1000.000000000000000 ) ;
#1787 = CARTESIAN_POINT ( 'NONE',  ( 6.972266317189433020E-16, -28.46875000068279959, -5.249999999999999112 ) ) ;
#1788 = CARTESIAN_POINT ( 'NONE',  ( 2.300847884672513123E-14, -28.18750000000000000, -5.250000000000000000 ) ) ;
#1789 = CARTESIAN_POINT ( 'NONE',  ( 3.616337804771879580E-16, -28.10937500034140157, -5.905927827173866440 ) ) ;
#1790 = VECTOR ( 'NONE', #7690, 1000.000000000000000 ) ;
#1791 = CARTESIAN_POINT ( 'NONE',  ( -2.007298707674168181, -4.858300672349188093E-16, 2.776755344285330107 ) ) ;
#1792 = CARTESIAN_POINT ( 'NONE',  ( 3.616337804771879580E-16, -27.29687500034139802, -5.905927827173866440 ) ) ;
#1793 = ORIENTED_EDGE ( 'NONE', *, *, #3059, .F. ) ;
#1794 = EDGE_CURVE ( 'NONE', #1056, #8492, #6936, .T. ) ;
#1795 = CARTESIAN_POINT ( 'NONE',  ( 5.249999999999999112, -27.85416666666666430, -3.031088913245536975 ) ) ;
#1796 = CARTESIAN_POINT ( 'NONE',  ( -5.385316468750000141, -28.60937499965860198, 0.000000000000000000 ) ) ;
#1797 = CARTESIAN_POINT ( 'NONE',  ( 1.406733260263394625, -29.94866454968462577, -5.250000000000000000 ) ) ;
#1798 = CARTESIAN_POINT ( 'NONE',  ( -5.385316468749998364, -29.58854166632527694, 3.109213912904140287 ) ) ;
#1799 = ORIENTED_EDGE ( 'NONE', *, *, #6925, .T. ) ;
#1800 = AXIS2_PLACEMENT_3D ( 'NONE', #2096, #4960, #5001 ) ;
#1801 = DIRECTION ( 'NONE',  ( 0.000000000000000000, 1.000000000000000000, 0.000000000000000000 ) ) ;
#1802 = CARTESIAN_POINT ( 'NONE',  ( 2.625000000000000444, -27.48958333401612819, -4.546633369868303021 ) ) ;
#1803 = CARTESIAN_POINT ( 'NONE',  ( -5.385316468750001029, -29.63020833299193768, -3.109213912904136734 ) ) ;
#1804 = UNCERTAINTY_MEASURE_WITH_UNIT (LENGTH_MEASURE( 1.000000000000000082E-05 ), #654, 'distance_accuracy_value', 'NONE');
#1805 = ADVANCED_FACE ( 'NONE', ( #1218 ), #5208, .T. ) ;
#1806 = ORIENTED_EDGE ( 'NONE', *, *, #6793, .F. ) ;
#1807 = VECTOR ( 'NONE', #8585, 1000.000000000000000 ) ;
#1808 = CARTESIAN_POINT ( 'NONE',  ( -5.385316468750001029, -27.84895833299193413, -3.109213912904136734 ) ) ;
#1809 = CARTESIAN_POINT ( 'NONE',  ( -3.492485675378566246, -1.450659073900639084, 1.467888652718973397 ) ) ;
#1810 = CARTESIAN_POINT ( 'NONE',  ( 2.300847884672513123E-14, -28.18750000000000000, -5.250000000000000000 ) ) ;
#1811 = SURFACE_SIDE_STYLE ('',( #1111 ) ) ;
#1812 = LINE ( 'NONE', #6268, #6422 ) ;
#1813 = CARTESIAN_POINT ( 'NONE',  ( 3.507514324621465285, -1.149340926099361226, -1.431606283892619347 ) ) ;
#1814 = CARTESIAN_POINT ( 'NONE',  ( 2.557341765625000818, -29.81770833367473372, -4.429445870380400052 ) ) ;
#1815 = DIRECTION ( 'NONE',  ( 0.000000000000000000, -1.000000000000000000, 0.000000000000000000 ) ) ;
#1816 = APPLICATION_PROTOCOL_DEFINITION ( 'draft international standard', 'automotive_design', 1998, #2733 ) ;
#1817 = CARTESIAN_POINT ( 'NONE',  ( 5.385316468750001029, -29.72395833299193413, 3.109213912904135846 ) ) ;
#1818 = CARTESIAN_POINT ( 'NONE',  ( 2.841254879263533262, -6.049340926099361582, -2.815599370228847320 ) ) ;
#1819 = DIRECTION ( 'NONE',  ( 0.000000000000000000, 0.000000000000000000, -1.000000000000000000 ) ) ;
#1820 = CARTESIAN_POINT ( 'NONE',  ( 2.692658234374998738, -28.66145833299193413, -4.663820869356206877 ) ) ;
#1821 = CARTESIAN_POINT ( 'NONE',  ( -3.507514324621434199, -4.450659073900639306, -1.431606283892695064 ) ) ;
#1822 = VERTEX_POINT ( 'NONE', #8975 ) ;
#1823 = CARTESIAN_POINT ( 'NONE',  ( 5.250000000000000000, -27.97916666666666430, -3.031088913245534755 ) ) ;
#1824 = FACE_OUTER_BOUND ( 'NONE', #8062, .T. ) ;
#1825 = CARTESIAN_POINT ( 'NONE',  ( -1.925759277493323207, -9.035843541029836168E-14, 2.922632427747480222 ) ) ;
#1826 = ORIENTED_EDGE ( 'NONE', *, *, #6824, .F. ) ;
#1827 = SHAPE_REPRESENTATION_RELATIONSHIP ( 'NONE' , 'NONE' ,  #1843, #2088 ) ;
#1828 = CARTESIAN_POINT ( 'NONE',  ( -3.712013335537174572E-16, -28.56249999999999645, -6.062177826491070398 ) ) ;
#1829 = VECTOR ( 'NONE', #8570, 1000.000000000000114 ) ;
#1830 = EDGE_LOOP ( 'NONE', ( #3630, #6617, #3382, #8852 ) ) ;
#1831 = APPLICATION_CONTEXT ( 'automotive_design' ) ;
#1832 = CARTESIAN_POINT ( 'NONE',  ( 5.114683531250000748, -28.60937500034139802, 0.000000000000000000 ) ) ;
#1833 = CARTESIAN_POINT ( 'NONE',  ( -2.108492589042306964, -1.649340926099361448, -2.134148098076978251 ) ) ;
#1834 = CYLINDRICAL_SURFACE ( 'NONE', #6978, 1.499999999999999778 ) ;
#1835 = CARTESIAN_POINT ( 'NONE',  ( 3.122849337825750419E-16, -53.00000000000000000, -2.549999999999999822 ) ) ;
#1836 = CARTESIAN_POINT ( 'NONE',  ( -5.114683531250000748, -29.27604166700806232, 2.952963913586931888 ) ) ;
#1837 = CARTESIAN_POINT ( 'NONE',  ( -2.625000000000000444, -29.22916666598386826, -4.546633369868303021 ) ) ;
#1838 = ADVANCED_FACE ( 'NONE', ( #1824 ), #564, .T. ) ;
#1839 = AXIS2_PLACEMENT_3D ( 'NONE', #1295, #9147, #511 ) ;
#1840 = AXIS2_PLACEMENT_3D ( 'NONE', #8431, #4287, #5630 ) ;
#1841 = CARTESIAN_POINT ( 'NONE',  ( 0.000000000000000000, -20.00000000000000000, 0.000000000000000000 ) ) ;
#1842 = CARTESIAN_POINT ( 'NONE',  ( 5.114683531249999859, -27.33854166700806232, -2.952963913586932776 ) ) ;
#1843 = SHAPE_REPRESENTATION ( 'dispenser', ( #888 ), #699 ) ;
#1844 = VERTEX_POINT ( 'NONE', #469 ) ;
#1845 = VECTOR ( 'NONE', #5986, 1000.000000000000000 ) ;
#1846 = LINE ( 'NONE', #8117, #3782 ) ;
#1847 = CARTESIAN_POINT ( 'NONE',  ( 2.692658234375002735, -28.77604166632526628, 4.663820869356205101 ) ) ;
#1848 = CARTESIAN_POINT ( 'NONE',  ( 0.000000000000000000, -27.00000000000000000, -5.250000000000000000 ) ) ;
#1849 = AXIS2_PLACEMENT_3D ( 'NONE', #1507, #3100, #159 ) ;
#1850 = CARTESIAN_POINT ( 'NONE',  ( 2.324088772396477476E-15, -27.49999999931720751, -5.250000000000000000 ) ) ;
#1851 = CARTESIAN_POINT ( 'NONE',  ( 5.385316468750001029, -30.00520833299193768, 3.109213912904135846 ) ) ;
#1852 = CARTESIAN_POINT ( 'NONE',  ( 0.01814118441321408565, -3.049340926099361138, -3.500000000000000000 ) ) ;
#1853 = ORIENTED_EDGE ( 'NONE', *, *, #2021, .F. ) ;
#1854 = DIRECTION ( 'NONE',  ( -0.000000000000000000, -1.000000000000000000, -0.000000000000000000 ) ) ;
#1855 = CARTESIAN_POINT ( 'NONE',  ( 2.624999999999996891, -28.32291666734946389, 4.546633369868304797 ) ) ;
#1856 = CARTESIAN_POINT ( 'NONE',  ( 2.692658234374998738, -28.69270833299193413, -4.663820869356206877 ) ) ;
#1857 = AXIS2_PLACEMENT_3D ( 'NONE', #1232, #7558, #8853 ) ;
#1858 = EDGE_LOOP ( 'NONE', ( #6387, #8496, #2011, #9019, #5652 ) ) ;
#1859 = EDGE_CURVE ( 'NONE', #3172, #2054, #418, .T. ) ;
#1860 = CARTESIAN_POINT ( 'NONE',  ( -2.692658234374996518, -27.78645833299193413, 4.663820869356208654 ) ) ;
#1861 = CARTESIAN_POINT ( 'NONE',  ( -3.000000000000000444, -7.750659073900639129, 0.01814118441314532468 ) ) ;
#1862 = DIRECTION ( 'NONE',  ( 1.000000000000000000, 0.000000000000000000, 0.000000000000000000 ) ) ;
#1863 = EDGE_CURVE ( 'NONE', #610, #27, #607, .T. ) ;
#1864 = SURFACE_SIDE_STYLE ('',( #404 ) ) ;
#1865 = CARTESIAN_POINT ( 'NONE',  ( 5.249999999999997335, -28.27083333333332860, 3.031088913245538308 ) ) ;
#1866 = CARTESIAN_POINT ( 'NONE',  ( 1.406733260263405061, -27.97991455036742181, -5.249999999999994671 ) ) ;
#1867 = ADVANCED_FACE ( 'NONE', ( #8196 ), #5538, .F. ) ;
#1868 = DIRECTION ( 'NONE',  ( 0.000000000000000000, -1.000000000000000000, 0.000000000000000000 ) ) ;
#1869 = ORIENTED_EDGE ( 'NONE', *, *, #7652, .T. ) ;
#1870 = SHAPE_DEFINITION_REPRESENTATION ( #2935, #2791 ) ;
#1871 = CARTESIAN_POINT ( 'NONE',  ( 2.692658234375002735, -29.49479166632526983, 4.663820869356205101 ) ) ;
#1872 = CARTESIAN_POINT ( 'NONE',  ( 0.01814118441321408565, -4.649340926099361226, -3.500000000000000000 ) ) ;
#1873 = DIRECTION ( 'NONE',  ( 0.000000000000000000, 1.000000000000000000, 0.000000000000000000 ) ) ;
#1874 = CARTESIAN_POINT ( 'NONE',  ( -3.807688866302469071E-16, -28.89062499965860198, -6.218427825808274356 ) ) ;
#1875 = CARTESIAN_POINT ( 'NONE',  ( -2.462045979635629323, -3.150659073900639040, 2.487701488670203798 ) ) ;
#1876 = EDGE_LOOP ( 'NONE', ( #7403, #4254, #2030, #5838 ) ) ;
#1877 = CARTESIAN_POINT ( 'NONE',  ( -2.624999999999996891, -30.14583333265053611, 4.546633369868304797 ) ) ;
#1878 = CARTESIAN_POINT ( 'NONE',  ( 0.000000000000000000, 70.00000000000000000, 0.000000000000000000 ) ) ;
#1879 = CARTESIAN_POINT ( 'NONE',  ( 2.557341765624996821, -26.96354166700806232, 4.429445870380401828 ) ) ;
#1880 = VERTEX_POINT ( 'NONE', #2710 ) ;
#1881 = SURFACE_STYLE_FILL_AREA ( #5445 ) ;
#1882 = CARTESIAN_POINT ( 'NONE',  ( 1.113604000661152470E-15, -27.93750000000000000, 6.062177826491070398 ) ) ;
#1883 = EDGE_LOOP ( 'NONE', ( #4980, #2956, #8311, #3672 ) ) ;
#1884 = CARTESIAN_POINT ( 'NONE',  ( -2.557341765624999042, -29.27604166700806232, -4.429445870380400052 ) ) ;
#1885 = CARTESIAN_POINT ( 'NONE',  ( 1.467888652719048226, -7.749340926099361759, -3.492485675378536047 ) ) ;
#1886 = DIRECTION ( 'NONE',  ( 0.000000000000000000, 1.000000000000000000, 0.000000000000000000 ) ) ;
#1887 = CARTESIAN_POINT ( 'NONE',  ( -2.557341765625002594, -27.75520833367473017, 4.429445870380399164 ) ) ;
#1888 = EDGE_CURVE ( 'NONE', #7866, #8580, #8382, .T. ) ;
#1889 = DIRECTION ( 'NONE',  ( 0.000000000000000000, 0.000000000000000000, -1.000000000000000000 ) ) ;
#1890 = CARTESIAN_POINT ( 'NONE',  ( -5.114683531250000748, -26.98437500034139802, -6.263680815196995234E-16 ) ) ;
#1891 = CARTESIAN_POINT ( 'NONE',  ( -5.114683531250000748, -29.27604166700806232, 2.952963913586931888 ) ) ;
#1892 = FACE_OUTER_BOUND ( 'NONE', #5432, .T. ) ;
#1893 = CARTESIAN_POINT ( 'NONE',  ( -5.385316468750001029, -29.13020833299193058, -3.109213912904136734 ) ) ;
#1894 = CARTESIAN_POINT ( 'NONE',  ( 0.000000000000000000, -20.00000000000000000, 0.000000000000000000 ) ) ;
#1895 = CARTESIAN_POINT ( 'NONE',  ( 1.142306659890740623E-15, -29.29687499965860198, 6.218427825808274356 ) ) ;
#1896 = CARTESIAN_POINT ( 'NONE',  ( 1.638713065079161924, -7.149340926099361226, 4.007514324621467949 ) ) ;
#1897 = ORIENTED_EDGE ( 'NONE', *, *, #7817, .F. ) ;
#1898 = CARTESIAN_POINT ( 'NONE',  ( 5.249999999999997335, -29.30208333401613174, 3.031088913245538308 ) ) ;
#1899 = CARTESIAN_POINT ( 'NONE',  ( 5.249999999999999112, -27.55208333401613174, 3.031088913245538308 ) ) ;
#1900 = CARTESIAN_POINT ( 'NONE',  ( -5.385316468750000141, -28.85937499965860198, 0.000000000000000000 ) ) ;
#1901 = ORIENTED_EDGE ( 'NONE', *, *, #957, .T. ) ;
#1902 = CARTESIAN_POINT ( 'NONE',  ( 5.385316468750001029, -28.22395833299193413, 3.109213912904134958 ) ) ;
#1903 = CARTESIAN_POINT ( 'NONE',  ( 0.01814118441313990887, -0.1506590739006389568, 3.500000000000000000 ) ) ;
#1904 = DIRECTION ( 'NONE',  ( 0.000000000000000000, -1.000000000000000000, 0.000000000000000000 ) ) ;
#1905 = MECHANICAL_DESIGN_GEOMETRIC_PRESENTATION_REPRESENTATION (  '', ( #9023 ), #3833 ) ;
#1906 = AXIS2_PLACEMENT_3D ( 'NONE', #2039, #6307, #4863 ) ;
#1907 = DIRECTION ( 'NONE',  ( 0.000000000000000000, 1.000000000000000000, 0.000000000000000000 ) ) ;
#1908 = CARTESIAN_POINT ( 'NONE',  ( -6.972266317189433020E-16, -28.49999999931720041, -5.250000000000000000 ) ) ;
#1909 = DIRECTION ( 'NONE',  ( -0.000000000000000000, 1.000000000000000000, -0.000000000000000000 ) ) ;
#1910 = DIRECTION ( 'NONE',  ( -0.000000000000000000, -1.000000000000000000, -0.000000000000000000 ) ) ;
#1911 = ORIENTED_EDGE ( 'NONE', *, *, #6017, .F. ) ;
#1912 = ITEM_DEFINED_TRANSFORMATION ( 'NONE', 'NONE', #7552,  #888 ) ;
#1913 = CARTESIAN_POINT ( 'NONE',  ( -2.692658234374996518, -30.03645833299193413, 4.663820869356208654 ) ) ;
#1914 = CARTESIAN_POINT ( 'NONE',  ( -3.507514324621464397, -3.549340926099361582, 1.431606283892619347 ) ) ;
#1915 = EDGE_CURVE ( 'NONE', #4653, #8235, #4037, .T. ) ;
#1916 = CARTESIAN_POINT ( 'NONE',  ( -2.624999999999996891, -29.45833333333333215, 4.546633369868304797 ) ) ;
#1917 = CARTESIAN_POINT ( 'NONE',  ( -2.692658234374996518, -30.03645833299193413, 4.663820869356208654 ) ) ;
#1918 = CARTESIAN_POINT ( 'NONE',  ( 3.507514324621434199, -3.650659073900639928, 1.431606283892693066 ) ) ;
#1919 = ORIENTED_EDGE ( 'NONE', *, *, #7197, .F. ) ;
#1920 = CARTESIAN_POINT ( 'NONE',  ( 1.406733300191166602, -30.01116454931871402, -5.249999976947688829 ) ) ;
#1921 = DIRECTION ( 'NONE',  ( -0.000000000000000000, -1.000000000000000000, -0.000000000000000000 ) ) ;
#1922 = CARTESIAN_POINT ( 'NONE',  ( -2.462045979635629323, -4.750659073900639129, 2.487701488670203798 ) ) ;
#1923 = EDGE_LOOP ( 'NONE', ( #2916, #7141, #653, #4705 ) ) ;
#1924 = CARTESIAN_POINT ( 'NONE',  ( -5.250000000000000000, -28.25000000000000000, 0.000000000000000000 ) ) ;
#1925 = ORIENTED_EDGE ( 'NONE', *, *, #6506, .T. ) ;
#1926 = VECTOR ( 'NONE', #6086, 1000.000000000000000 ) ;
#1927 = CARTESIAN_POINT ( 'NONE',  ( 2.557341765625000818, -28.56770833367473017, -4.429445870380400052 ) ) ;
#1928 = CARTESIAN_POINT ( 'NONE',  ( 2.992485675378538712, -2.549340926099361582, 1.260781871532494103 ) ) ;
#1929 = DIRECTION ( 'NONE',  ( 0.000000000000000000, 1.000000000000000000, 0.000000000000000000 ) ) ;
#1930 = CARTESIAN_POINT ( 'NONE',  ( -1.084901341431563923E-15, -26.98437500034139802, 5.905927827173866440 ) ) ;
#1931 = FACE_BOUND ( 'NONE', #7456, .T. ) ;
#1932 = CARTESIAN_POINT ( 'NONE',  ( -5.114683531250000748, -27.23437500034139802, -6.263680815196995234E-16 ) ) ;
#1933 = AXIS2_PLACEMENT_3D ( 'NONE', #8132, #6540, #1008 ) ;
#1934 = CARTESIAN_POINT ( 'NONE',  ( 5.250000000000000000, -27.00000000000000000, 0.000000000000000000 ) ) ;
#1935 = CARTESIAN_POINT ( 'NONE',  ( 5.114683531249998971, -28.44270833367473017, 2.952963913586936329 ) ) ;
#1936 = DIRECTION ( 'NONE',  ( 0.000000000000000000, 1.000000000000000000, 0.000000000000000000 ) ) ;
#1937 = CARTESIAN_POINT ( 'NONE',  ( -5.385316468750000141, -28.35937499965860198, 0.000000000000000000 ) ) ;
#1938 = DIRECTION ( 'NONE',  ( 0.000000000000000000, -0.000000000000000000, 1.000000000000000000 ) ) ;
#1939 = CARTESIAN_POINT ( 'NONE',  ( 5.385316468750000141, -29.98437499965859843, -6.595110575850215044E-16 ) ) ;
#1940 = CARTESIAN_POINT ( 'NONE',  ( -3.500000000000000000, -0.2493409260993610654, -0.01814118441321344033 ) ) ;
#1941 = COLOUR_RGB ( '',0.8941176470588234615, 0.8941176470588234615, 0.8941176470588234615 ) ;
#1942 = CARTESIAN_POINT ( 'NONE',  ( 1.467888652719048226, -2.949340926099361493, -3.492485675378536047 ) ) ;
#1943 = VERTEX_POINT ( 'NONE', #6193 ) ;
#1944 = CARTESIAN_POINT ( 'NONE',  ( 0.000000000000000000, -35.00000000000000000, 0.000000000000000000 ) ) ;
#1945 = CARTESIAN_POINT ( 'NONE',  ( -1.113604000661152470E-15, -28.59375000068279604, 6.062177826491070398 ) ) ;
#1946 = CARTESIAN_POINT ( 'NONE',  ( 5.385316468750000141, -28.98437499965859843, -6.595110575850215044E-16 ) ) ;
#1947 = ORIENTED_EDGE ( 'NONE', *, *, #7078, .F. ) ;
#1948 = CARTESIAN_POINT ( 'NONE',  ( 2.692658234374998738, -28.66145833299193413, -4.663820869356206877 ) ) ;
#1949 = CARTESIAN_POINT ( 'NONE',  ( -3.507514324621434199, -1.250659073900638907, -1.431606283892695064 ) ) ;
#1950 = CARTESIAN_POINT ( 'NONE',  ( 3.061616997868383634E-16, -20.00000000000000000, -2.500000000000000444 ) ) ;
#1951 = CIRCLE ( 'NONE', #295, 0.2499999999999998335 ) ;
#1952 =( BOUNDED_CURVE ( )  B_SPLINE_CURVE ( 2, ( #7631, #3960, #9065, #5484, #3358, #7677, #4006, #4740, #9016 ),
 .UNSPECIFIED., .F., .F. ) 
 B_SPLINE_CURVE_WITH_KNOTS ( ( 3, 2, 2, 2, 3 ),
 ( 0.4375000000000000000, 0.4444444444444444198, 0.4583333333333333148, 0.4722222222222222099, 0.4791666666666666852 ),
 .UNSPECIFIED. ) 
 CURVE ( )  GEOMETRIC_REPRESENTATION_ITEM ( )  RATIONAL_B_SPLINE_CURVE ( ( 0.9330127018922194093, 0.9330127018922194093, 1.000000000000000000, 0.8660254037844387076, 1.000000000000000000, 0.8660254037844387076, 1.000000000000000000, 0.9330127018922190762, 0.9330127018922194093 ) ) 
 REPRESENTATION_ITEM ( '' )  );
#1953 = ADVANCED_FACE ( 'NONE', ( #6094 ), #2666, .F. ) ;
#1954 = FACE_OUTER_BOUND ( 'NONE', #5271, .T. ) ;
#1955 = CARTESIAN_POINT ( 'NONE',  ( 1.406733260263403507, -28.82366454968462222, -5.249999999999994671 ) ) ;
#1956 = AXIS2_PLACEMENT_3D ( 'NONE', #1124, #8287, #2575 ) ;
#1957 = CARTESIAN_POINT ( 'NONE',  ( 0.000000000000000000, -53.00000000000000000, 0.000000000000000000 ) ) ;
#1958 = DIRECTION ( 'NONE',  ( 0.000000000000000000, 0.000000000000000000, -1.000000000000000000 ) ) ;
#1959 = PRODUCT_CONTEXT ( 'NONE', #8129, 'mechanical' ) ;
#1960 = CARTESIAN_POINT ( 'NONE',  ( -5.385316468749998364, -29.55729166632526983, 3.109213912904140287 ) ) ;
#1961 = CARTESIAN_POINT ( 'NONE',  ( 3.500000000000000000, -4.249340926099360871, 0.01814118441321387054 ) ) ;
#1962 = CARTESIAN_POINT ( 'NONE',  ( 1.836970198721030181E-16, 70.00000000000000000, 1.500000000000000222 ) ) ;
#1963 = CARTESIAN_POINT ( 'NONE',  ( -5.385316468750001029, -27.13020833299193413, -3.109213912904136734 ) ) ;
#1964 = CARTESIAN_POINT ( 'NONE',  ( 3.492485675378566690, -3.850659073900639218, -1.467888652718972287 ) ) ;
#1965 = CARTESIAN_POINT ( 'NONE',  ( -5.250000000000000000, -30.18749999931720041, 0.000000000000000000 ) ) ;
#1966 = DIRECTION ( 'NONE',  ( 0.000000000000000000, 0.000000000000000000, -1.000000000000000000 ) ) ;
#1967 = VERTEX_POINT ( 'NONE', #5393 ) ;
#1968 = CARTESIAN_POINT ( 'NONE',  ( 5.250000000000000888, -28.64583333333332860, 3.031088913245532979 ) ) ;
#1969 = CARTESIAN_POINT ( 'NONE',  ( 5.114683531250000748, -27.83854166700806587, -2.952963913586932776 ) ) ;
#1970 = CARTESIAN_POINT ( 'NONE',  ( -3.007514324621463508, -1.949340926099361493, 1.224499502706077658 ) ) ;
#1971 = LINE ( 'NONE', #4800, #4797 ) ;
#1972 = CARTESIAN_POINT ( 'NONE',  ( -2.557341765624999042, -27.83854166700806587, -4.429445870380400052 ) ) ;
#1973 = LINE ( 'NONE', #8985, #1381 ) ;
#1974 = CARTESIAN_POINT ( 'NONE',  ( -2.557341765624999042, -29.83854166700806232, -4.429445870380400052 ) ) ;
#1975 = ADVANCED_FACE ( 'NONE', ( #1264, #5489 ), #4702, .T. ) ;
#1976 = CARTESIAN_POINT ( 'NONE',  ( 2.557341765625000818, -28.88020833367473017, -4.429445870380400052 ) ) ;
#1977 = CARTESIAN_POINT ( 'NONE',  ( -2.625000000000002220, -28.36458333401612819, 4.546633369868302132 ) ) ;
#1978 = CARTESIAN_POINT ( 'NONE',  ( -3.712013335537174572E-16, -28.99999999931720751, -6.062177826491070398 ) ) ;
#1979 = LINE ( 'NONE', #1848, #3459 ) ;
#1980 = CARTESIAN_POINT ( 'NONE',  ( -3.431411822166540393, -3.932028342760356289E-17, 1.490417237447617449 ) ) ;
#1981 = CARTESIAN_POINT ( 'NONE',  ( -5.385316468750001029, -29.88020833299193413, -3.109213912904136734 ) ) ;
#1982 = CARTESIAN_POINT ( 'NONE',  ( -1.638713065079163034, -7.949340926099362825, -4.007514324621466173 ) ) ;
#1983 = CARTESIAN_POINT ( 'NONE',  ( -3.507514324621464397, -0.3493409260993610710, 1.431606283892619347 ) ) ;
#1984 = AXIS2_PLACEMENT_3D ( 'NONE', #2199, #5726, #3555 ) ;
#1985 = ORIENTED_EDGE ( 'NONE', *, *, #8607, .F. ) ;
#1986 = DIRECTION ( 'NONE',  ( 0.000000000000000000, 0.000000000000000000, -1.000000000000000000 ) ) ;
#1987 = CARTESIAN_POINT ( 'NONE',  ( -2.557341765624999042, -29.52604166700806232, -4.429445870380400052 ) ) ;
#1988 = B_SPLINE_CURVE_WITH_KNOTS ( 'NONE', 3,
 ( #6414, #7, #8480, #2810 ),
 .UNSPECIFIED., .F., .F.,
 ( 4, 4 ),
 ( 0.008580651465885628590, 0.01459740681124464291 ),
 .UNSPECIFIED. ) ;
#1989 = CARTESIAN_POINT ( 'NONE',  ( -2.692658234375000514, -28.90104166632526983, -4.663820869356205989 ) ) ;
#1990 = AXIS2_PLACEMENT_3D ( 'NONE', #8461, #2087, #4227 ) ;
#1991 = AXIS2_PLACEMENT_3D ( 'NONE', #8111, #944, #8759 ) ;
#1992 = ORIENTED_EDGE ( 'NONE', *, *, #2626, .F. ) ;
#1993 = DIRECTION ( 'NONE',  ( 0.000000000000000000, -1.000000000000000000, 0.000000000000000000 ) ) ;
#1994 = CARTESIAN_POINT ( 'NONE',  ( -1.467888652718973619, -2.650659073900639040, -3.492485675378565801 ) ) ;
#1995 = DIRECTION ( 'NONE',  ( 0.000000000000000000, 0.000000000000000000, -1.000000000000000000 ) ) ;
#1996 = CIRCLE ( 'NONE', #506, 5.250000000000000000 ) ;
#1997 = FILL_AREA_STYLE_COLOUR ( '', #7726 ) ;
#1998 = DIRECTION ( 'NONE',  ( 0.000000000000000000, 0.000000000000000000, 1.000000000000000000 ) ) ;
#1999 = CARTESIAN_POINT ( 'NONE',  ( -1.467888652719046449, -6.949340926099361049, 3.492485675378535603 ) ) ;
#2000 = CARTESIAN_POINT ( 'NONE',  ( -2.557341765624999042, -28.52604166700806587, -4.429445870380400052 ) ) ;
#2001 = CARTESIAN_POINT ( 'NONE',  ( 0.000000000000000000, 81.00000000000001421, 0.000000000000000000 ) ) ;
#2002 = APPLICATION_PROTOCOL_DEFINITION ( 'draft international standard', 'automotive_design', 1998, #1268 ) ;
#2003 = CARTESIAN_POINT ( 'NONE',  ( 5.385316468749999252, -29.18229166632526983, -3.109213912904139399 ) ) ;
#2004 = CARTESIAN_POINT ( 'NONE',  ( -1.431606283892620235, -7.949340926099361049, -3.507514324621463953 ) ) ;
#2005 =( BOUNDED_CURVE ( )  B_SPLINE_CURVE ( 2, ( #3831, #5964, #7361, #4431, #5169, #102, #4388, #2953, #1547 ),
 .UNSPECIFIED., .F., .T. ) 
 B_SPLINE_CURVE_WITH_KNOTS ( ( 3, 2, 2, 2, 3 ),
 ( 0.7708333333333332593, 0.7777777777777777901, 0.7916666666666666297, 0.8055555555555555802, 0.8125000000000000000 ),
 .UNSPECIFIED. ) 
 CURVE ( )  GEOMETRIC_REPRESENTATION_ITEM ( )  RATIONAL_B_SPLINE_CURVE ( ( 0.9330127018922192983, 0.9330127018922187432, 1.000000000000000000, 0.8660254037844387076, 1.000000000000000000, 0.8660254037844387076, 1.000000000000000000, 0.9330127018922194093, 0.9330127018922194093 ) ) 
 REPRESENTATION_ITEM ( '' )  );
#2006 = CARTESIAN_POINT ( 'NONE',  ( 1.045839947578414884E-14, -28.06249999999999289, -5.250000000000000000 ) ) ;
#2007 = CARTESIAN_POINT ( 'NONE',  ( 5.385316468750000141, -27.23437499965860198, -6.595110575850215044E-16 ) ) ;
#2008 = CARTESIAN_POINT ( 'NONE',  ( -3.992485675378568022, -1.450659073900638862, 1.674995433905515529 ) ) ;
#2009 = LINE ( 'NONE', #3362, #3473 ) ;
#2010 = CARTESIAN_POINT ( 'NONE',  ( 0.000000000000000000, -30.00000000000000000, 0.000000000000000000 ) ) ;
#2011 = ORIENTED_EDGE ( 'NONE', *, *, #872, .T. ) ;
#2012 = SURFACE_STYLE_USAGE ( .BOTH. , #6196 ) ;
#2013 = CARTESIAN_POINT ( 'NONE',  ( -3.712013335537174572E-16, -28.06250000000000000, -6.062177826491070398 ) ) ;
#2014 = CARTESIAN_POINT ( 'NONE',  ( -5.114683531250001636, -27.96354166700806587, 2.952963913586931444 ) ) ;
#2015 = CARTESIAN_POINT ( 'NONE',  ( 2.108492589042307408, -5.649340926099361226, 2.134148098076978251 ) ) ;
#2016 = CARTESIAN_POINT ( 'NONE',  ( -1.084901341431563923E-15, -27.98437500034139802, 5.905927827173866440 ) ) ;
#2017 = CARTESIAN_POINT ( 'NONE',  ( 0.000000000000000000, 69.99999999999998579, 6.250000000000000000 ) ) ;
#2018 = EDGE_CURVE ( 'NONE', #3890, #7425, #4835, .T. ) ;
#2019 = CARTESIAN_POINT ( 'NONE',  ( 3.616337804771879580E-16, -28.60937500034139802, -5.905927827173866440 ) ) ;
#2020 = CARTESIAN_POINT ( 'NONE',  ( -5.114683531249999859, -28.56770833367473017, -2.952963913586935440 ) ) ;
#2021 = EDGE_CURVE ( 'NONE', #1822, #7425, #5506, .T. ) ;
#2022 = CARTESIAN_POINT ( 'NONE',  ( 0.000000000000000000, -27.00000000000000000, 0.000000000000000000 ) ) ;
#2023 = CARTESIAN_POINT ( 'NONE',  ( -5.250000000000000000, -28.68749999931720396, 0.000000000000000000 ) ) ;
#2024 = FACE_OUTER_BOUND ( 'NONE', #4217, .T. ) ;
#2025 = EDGE_CURVE ( 'NONE', #7863, #6101, #7202, .T. ) ;
#2026 =( NAMED_UNIT ( * ) PLANE_ANGLE_UNIT ( ) SI_UNIT ( $, .RADIAN. ) );
#2027 = CARTESIAN_POINT ( 'NONE',  ( 0.000000000000000000, -28.00000000000000000, 0.000000000000000000 ) ) ;
#2028 = CARTESIAN_POINT ( 'NONE',  ( 2.487701488670255756, -4.449340926099361937, -2.462045979635577364 ) ) ;
#2029 = CARTESIAN_POINT ( 'NONE',  ( -4.000000000000000000, -8.249340926099360871, -0.01814118441321865144 ) ) ;
#2030 = ORIENTED_EDGE ( 'NONE', *, *, #7078, .T. ) ;
#2031 = CARTESIAN_POINT ( 'NONE',  ( 9.180150650966086169E-15, -28.81249999999999645, 5.249999999999999112 ) ) ;
#2032 = CARTESIAN_POINT ( 'NONE',  ( -2.557341765625002594, -29.44270833367473017, 4.429445870380399164 ) ) ;
#2033 = CARTESIAN_POINT ( 'NONE',  ( 2.692658234374998738, -29.94270833299193413, -4.663820869356206877 ) ) ;
#2034 = ORIENTED_EDGE ( 'NONE', *, *, #3389, .F. ) ;
#2035 = CARTESIAN_POINT ( 'NONE',  ( -5.385316468749998364, -29.55729166632526983, 3.109213912904140287 ) ) ;
#2036 = CARTESIAN_POINT ( 'NONE',  ( -3.507514324621434199, -7.650659073900639484, -1.431606283892695064 ) ) ;
#2037 = CARTESIAN_POINT ( 'NONE',  ( 6.429395695523604153E-16, -27.00000000000000000, 5.250000000000000000 ) ) ;
#2038 = CARTESIAN_POINT ( 'NONE',  ( -5.249999999999997335, -28.97916666666666430, 3.031088913245538308 ) ) ;
#2039 = CARTESIAN_POINT ( 'NONE',  ( 0.000000000000000000, 0.000000000000000000, 0.000000000000000000 ) ) ;
#2040 = DIRECTION ( 'NONE',  ( 0.000000000000000000, 0.000000000000000000, -1.000000000000000000 ) ) ;
#2041 = CARTESIAN_POINT ( 'NONE',  ( -5.114683531249999859, -28.00520833367473017, -2.952963913586935440 ) ) ;
#2042 = CARTESIAN_POINT ( 'NONE',  ( 1.406733260263390628, -28.36383544963256753, 5.250000000000001776 ) ) ;
#2043 = DIRECTION ( 'NONE',  ( 0.000000000000000000, 0.000000000000000000, 1.000000000000000000 ) ) ;
#2044 = EDGE_CURVE ( 'NONE', #7888, #784, #2073, .T. ) ;
#2045 = CARTESIAN_POINT ( 'NONE',  ( -3.000000000000000444, -6.649340926099362115, -0.01814118441320822922 ) ) ;
#2046 = CARTESIAN_POINT ( 'NONE',  ( -5.250000000000000000, -28.15625000068279604, -6.429395695523604153E-16 ) ) ;
#2047 = CARTESIAN_POINT ( 'NONE',  ( 2.692658234374998738, -29.16145833299193413, -4.663820869356206877 ) ) ;
#2048 = ADVANCED_FACE ( 'NONE', ( #5666, #2848 ), #4235, .F. ) ;
#2049 = CARTESIAN_POINT ( 'NONE',  ( -0.01814118441313417734, -4.150659073900638596, -4.000000000000000000 ) ) ;
#2050 = CARTESIAN_POINT ( 'NONE',  ( 0.000000000000000000, -28.00000000000000000, 0.000000000000000000 ) ) ;
#2051 = CARTESIAN_POINT ( 'NONE',  ( 2.624999999999996891, -27.29166666666666430, 4.546633369868304797 ) ) ;
#2052 = CARTESIAN_POINT ( 'NONE',  ( -1.922037972912167048, -5.459919674189117688E-16, 2.905699108924820084 ) ) ;
#2053 =( GEOMETRIC_REPRESENTATION_CONTEXT ( 3 ) GLOBAL_UNCERTAINTY_ASSIGNED_CONTEXT ( ( #860 ) ) GLOBAL_UNIT_ASSIGNED_CONTEXT ( ( #473, #3318, #6899 ) ) REPRESENTATION_CONTEXT ( 'NONE', 'WORKASPACE' ) );
#2054 = VERTEX_POINT ( 'NONE', #2139 ) ;
#2055 = CARTESIAN_POINT ( 'NONE',  ( -2.624999999999996891, -29.70833333333333215, 4.546633369868304797 ) ) ;
#2056 = CARTESIAN_POINT ( 'NONE',  ( 2.557341765624996821, -27.15104166700806587, 4.429445870380401828 ) ) ;
#2057 = CARTESIAN_POINT ( 'NONE',  ( -3.000000000000000444, -2.950659073900639306, 0.01814118441314532468 ) ) ;
#2058 = CARTESIAN_POINT ( 'NONE',  ( 2.557341765625000818, -27.63020833367473017, -4.429445870380400052 ) ) ;
#2059 = CARTESIAN_POINT ( 'NONE',  ( -5.114683531250000748, -28.56770833367473017, -2.952963913586935440 ) ) ;
#2060 = LINE ( 'NONE', #2770, #1790 ) ;
#2061 = CARTESIAN_POINT ( 'NONE',  ( -5.114683531250000748, -29.54687500034139802, -6.263680815196995234E-16 ) ) ;
#2062 = CARTESIAN_POINT ( 'NONE',  ( 9.180150650966086169E-15, -28.34375000068279604, 5.250000000000000000 ) ) ;
#2063 = CARTESIAN_POINT ( 'NONE',  ( -5.250000000000000000, -29.18749999931720396, 0.000000000000000000 ) ) ;
#2064 = DIRECTION ( 'NONE',  ( 0.000000000000000000, 1.000000000000000000, 0.000000000000000000 ) ) ;
#2065 = DIRECTION ( 'NONE',  ( 0.000000000000000000, 1.000000000000000000, 0.000000000000000000 ) ) ;
#2066 = CARTESIAN_POINT ( 'NONE',  ( -1.431606283892620235, -4.749340926099363536, -3.507514324621463953 ) ) ;
#2067 = CARTESIAN_POINT ( 'NONE',  ( -1.467888652719046449, -5.349340926099361404, 3.492485675378536047 ) ) ;
#2068 = EDGE_LOOP ( 'NONE', ( #4434, #51, #3698, #1603 ) ) ;
#2069 = VECTOR ( 'NONE', #7469, 1000.000000000000000 ) ;
#2070 = CARTESIAN_POINT ( 'NONE',  ( -5.249999999999999112, -29.70833333265053611, -3.031088913245534755 ) ) ;
#2071 = CARTESIAN_POINT ( 'NONE',  ( 2.557341765625000818, -29.56770833367473017, -4.429445870380400052 ) ) ;
#2072 = EDGE_CURVE ( 'NONE', #1130, #187, #3438, .T. ) ;
#2073 =( BOUNDED_CURVE ( )  B_SPLINE_CURVE ( 2, ( #4322, #4876, #2051, #2353, #7724, #2180, #2892, #8595, #7815 ),
 .UNSPECIFIED., .F., .T. ) 
 B_SPLINE_CURVE_WITH_KNOTS ( ( 3, 2, 2, 2, 3 ),
 ( 0.8958333333333333703, 0.9027777777777777901, 0.9166666666666666297, 0.9305555555555555802, 0.9375000000000000000 ),
 .UNSPECIFIED. ) 
 CURVE ( )  GEOMETRIC_REPRESENTATION_ITEM ( )  RATIONAL_B_SPLINE_CURVE ( ( 0.9330127018922192983, 0.9330127018922198534, 1.000000000000000000, 0.8660254037844387076, 1.000000000000000000, 0.8660254037844387076, 1.000000000000000000, 0.9330127018922194093, 0.9330127018922194093 ) ) 
 REPRESENTATION_ITEM ( '' )  );
#2074 = VERTEX_POINT ( 'NONE', #2226 ) ;
#2075 = AXIS2_PLACEMENT_3D ( 'NONE', #893, #5822, #7966 ) ;
#2076 = CARTESIAN_POINT ( 'NONE',  ( -2.692658234375000514, -29.11979166632526983, -4.663820869356205989 ) ) ;
#2077 = CARTESIAN_POINT ( 'NONE',  ( -3.992485675378568022, -1.450659073900638862, 1.674995433905515529 ) ) ;
#2078 = LINE ( 'NONE', #9180, #1470 ) ;
#2079 = AXIS2_PLACEMENT_3D ( 'NONE', #1001, #1561, #6628 ) ;
#2080 = ORIENTED_EDGE ( 'NONE', *, *, #5233, .F. ) ;
#2081 = CARTESIAN_POINT ( 'NONE',  ( -1.406733260263395735, -27.57366454968463287, 5.250000000000000000 ) ) ;
#2082 = DIRECTION ( 'NONE',  ( 0.000000000000000000, 0.000000000000000000, -1.000000000000000000 ) ) ;
#2083 = VECTOR ( 'NONE', #6598, 1000.000000000000000 ) ;
#2084 = EDGE_CURVE ( 'NONE', #5960, #5957, #3878, .T. ) ;
#2085 = CARTESIAN_POINT ( 'NONE',  ( 5.249999999999999112, -27.29166666598386826, -3.031088913245536975 ) ) ;
#2086 = CARTESIAN_POINT ( 'NONE',  ( 5.114683531249999859, -29.08854166700806942, -2.952963913586932776 ) ) ;
#2087 = DIRECTION ( 'NONE',  ( 0.000000000000000000, -1.000000000000000000, 0.000000000000000000 ) ) ;
#2088 = ADVANCED_BREP_SHAPE_REPRESENTATION ( '', ( #5133, #888 ), #699 ) ;
#2089 = CARTESIAN_POINT ( 'NONE',  ( -1.406733260263397289, -28.63616454900182973, 5.249999999999997335 ) ) ;
#2090 = EDGE_CURVE ( 'NONE', #7322, #874, #8621, .T. ) ;
#2091 = CARTESIAN_POINT ( 'NONE',  ( 2.992485675378538712, -5.749340926099361759, 1.260781871532494103 ) ) ;
#2092 = CARTESIAN_POINT ( 'NONE',  ( 5.250000000000000888, -28.64583333333332860, 3.031088913245533423 ) ) ;
#2093 = CARTESIAN_POINT ( 'NONE',  ( -5.385316468750000141, -29.07812499965860198, 0.000000000000000000 ) ) ;
#2094 = CARTESIAN_POINT ( 'NONE',  ( 3.992485675378568910, -3.850659073900639662, -1.674995433905514863 ) ) ;
#2095 = AXIS2_PLACEMENT_3D ( 'NONE', #5123, #4435, #8712 ) ;
#2096 = CARTESIAN_POINT ( 'NONE',  ( 0.000000000000000000, -50.00000000000000000, 0.000000000000000000 ) ) ;
#2097 = CARTESIAN_POINT ( 'NONE',  ( 6.972266317189433020E-16, -26.96875000068279249, -5.250000000000000000 ) ) ;
#2098 = ORIENTED_EDGE ( 'NONE', *, *, #6789, .T. ) ;
#2099 = CARTESIAN_POINT ( 'NONE',  ( -2.624999999999996891, -29.20833333333333215, 4.546633369868304797 ) ) ;
#2100 = ORIENTED_EDGE ( 'NONE', *, *, #2072, .T. ) ;
#2101 = CARTESIAN_POINT ( 'NONE',  ( -2.557341765625002594, -27.44270833367473017, 4.429445870380399164 ) ) ;
#2102 = CARTESIAN_POINT ( 'NONE',  ( 2.992485675378538712, -7.349340926099363180, 1.260781871532494103 ) ) ;
#2103 = CARTESIAN_POINT ( 'NONE',  ( 5.250000000000000000, -28.72916666666666785, -3.031088913245534755 ) ) ;
#2104 = CARTESIAN_POINT ( 'NONE',  ( -5.385316468750000141, -30.09374999965860198, 0.000000000000000000 ) ) ;
#2105 = CARTESIAN_POINT ( 'NONE',  ( -5.114683531250000748, -29.29687500034139802, -6.263680815196995234E-16 ) ) ;
#2106 = CARTESIAN_POINT ( 'NONE',  ( 2.557341765624996821, -27.21354166700806587, 4.429445870380401828 ) ) ;
#2107 = CARTESIAN_POINT ( 'NONE',  ( -5.250000000000000000, -29.20833333265053611, -3.031088913245534755 ) ) ;
#2108 = PRODUCT ( 'dispenser ring', 'dispenser ring', '', ( #1959 ) ) ;
#2109 = CARTESIAN_POINT ( 'NONE',  ( 0.000000000000000000, -27.00000000000000000, -5.250000000000000000 ) ) ;
#2110 = CARTESIAN_POINT ( 'NONE',  ( 1.406733260263393070, -29.47991455036742181, -5.250000000000000888 ) ) ;
#2111 = CARTESIAN_POINT ( 'NONE',  ( 2.624999999999996891, -28.54166666666666785, 4.546633369868304797 ) ) ;
#2112 = CARTESIAN_POINT ( 'NONE',  ( -1.467888652719046449, -2.149340926099360782, 3.492485675378536047 ) ) ;
#2113 = CARTESIAN_POINT ( 'NONE',  ( -3.492485675378536047, -3.349340926099361404, -1.467888652719048670 ) ) ;
#2114 = EDGE_LOOP ( 'NONE', ( #6518, #6060, #376, #5968 ) ) ;
#2115 = CARTESIAN_POINT ( 'NONE',  ( 1.975475456537005874E-15, -28.87499999931720396, 5.250000000000000000 ) ) ;
#2116 = CARTESIAN_POINT ( 'NONE',  ( -2.624999999999998668, -27.19791666734946389, -4.546633369868303021 ) ) ;
#2117 = VERTEX_POINT ( 'NONE', #2933 ) ;
#2118 = AXIS2_PLACEMENT_3D ( 'NONE', #2001, #7761, #2656 ) ;
#2119 = CARTESIAN_POINT ( 'NONE',  ( 5.385316468750001029, -28.97395833299193413, 3.109213912904134958 ) ) ;
#2120 = CARTESIAN_POINT ( 'NONE',  ( -1.638713065079245634, -1.650659073900638818, 4.007514324621432422 ) ) ;
#2121 = CARTESIAN_POINT ( 'NONE',  ( 0.000000000000000000, 75.00000000000000000, 0.000000000000000000 ) ) ;
#2122 = VERTEX_POINT ( 'NONE', #689 ) ;
#2123 = CARTESIAN_POINT ( 'NONE',  ( -1.406733260263394625, -29.05133545031537068, -5.250000000000000000 ) ) ;
#2124 = AXIS2_PLACEMENT_3D ( 'NONE', #5746, #4267, #3573 ) ;
#2125 = DIRECTION ( 'NONE',  ( -0.000000000000000000, -1.000000000000000000, -0.000000000000000000 ) ) ;
#2126 =( BOUNDED_CURVE ( )  B_SPLINE_CURVE ( 2, ( #8324, #2562, #9009, #9057, #8372, #2654, #7485, #1866, #7580 ),
 .UNSPECIFIED., .F., .F. ) 
 B_SPLINE_CURVE_WITH_KNOTS ( ( 3, 2, 2, 2, 3 ),
 ( 0.5625000000000000000, 0.5694444444444444198, 0.5833333333333333703, 0.5972222222222222099, 0.6041666666666666297 ),
 .UNSPECIFIED. ) 
 CURVE ( )  GEOMETRIC_REPRESENTATION_ITEM ( )  RATIONAL_B_SPLINE_CURVE ( ( 0.9330127018922194093, 0.9330127018922194093, 1.000000000000000000, 0.8660254037844387076, 1.000000000000000000, 0.8660254037844387076, 1.000000000000000000, 0.9330127018922198534, 0.9330127018922192983 ) ) 
 REPRESENTATION_ITEM ( '' )  );
#2127 = CARTESIAN_POINT ( 'NONE',  ( -3.807688866302469071E-16, -27.17187499965860198, -6.218427825808274356 ) ) ;
#2128 = EDGE_CURVE ( 'NONE', #7091, #4744, #5796, .T. ) ;
#2129 = CARTESIAN_POINT ( 'NONE',  ( -1.084901341431563923E-15, -28.42187500034139802, 5.905927827173866440 ) ) ;
#2130 = CARTESIAN_POINT ( 'NONE',  ( -5.250000000000000000, -28.18749999931720396, 0.000000000000000000 ) ) ;
#2131 = MANIFOLD_SOLID_BREP ( 'Thread1', #7871 ) ;
#2132 = LINE ( 'NONE', #2219, #201 ) ;
#2133 = CARTESIAN_POINT ( 'NONE',  ( -3.007514324621463508, -3.549340926099361582, 1.224499502706077658 ) ) ;
#2134 = ADVANCED_FACE ( 'NONE', ( #3493 ), #5635, .F. ) ;
#2135 = FACE_OUTER_BOUND ( 'NONE', #5491, .T. ) ;
#2136 = CARTESIAN_POINT ( 'NONE',  ( 5.385316468750001029, -28.50520833299193058, 3.109213912904135846 ) ) ;
#2137 = CARTESIAN_POINT ( 'NONE',  ( 2.841254879263473310, -5.150659073900639484, 2.815599370228907272 ) ) ;
#2138 = VECTOR ( 'NONE', #7889, 1000.000000000000000 ) ;
#2139 = CARTESIAN_POINT ( 'NONE',  ( -1.975475456537005874E-15, -28.31249999999999645, 5.249999999999999112 ) ) ;
#2140 = ADVANCED_FACE ( 'NONE', ( #5620, #83 ), #8469, .F. ) ;
#2141 = CARTESIAN_POINT ( 'NONE',  ( -5.250000000000000000, -27.87500000000000000, -6.429395695523604153E-16 ) ) ;
#2142 = VERTEX_POINT ( 'NONE', #1392 ) ;
#2143 = SURFACE_STYLE_USAGE ( .BOTH. , #1396 ) ;
#2144 = CARTESIAN_POINT ( 'NONE',  ( -5.385316468750000141, -27.07812499965860198, 0.000000000000000000 ) ) ;
#2145 = ORIENTED_EDGE ( 'NONE', *, *, #4082, .T. ) ;
#2146 = CARTESIAN_POINT ( 'NONE',  ( 5.114683531249998971, -27.38020833367473372, 2.952963913586936329 ) ) ;
#2147 = CARTESIAN_POINT ( 'NONE',  ( -2.134148098076978251, -6.849340926099361404, 2.108492589042307408 ) ) ;
#2148 = MANIFOLD_SOLID_BREP ( 'Boss-Extrude1', #7133 ) ;
#2149 = CARTESIAN_POINT ( 'NONE',  ( -5.250000000000000888, -29.35416666666666430, 3.031088913245532979 ) ) ;
#2150 = CARTESIAN_POINT ( 'NONE',  ( 2.625000000000002220, -29.41666666666666785, 4.546633369868302132 ) ) ;
#2151 = CARTESIAN_POINT ( 'NONE',  ( 5.114683531250000748, -28.67187500034139802, 0.000000000000000000 ) ) ;
#2152 =( LENGTH_UNIT ( ) NAMED_UNIT ( * ) SI_UNIT ( .MILLI., .METRE. ) );
#2153 = CARTESIAN_POINT ( 'NONE',  ( 5.114683531249998971, -28.19270833367473372, 2.952963913586936329 ) ) ;
#2154 = EDGE_CURVE ( 'NONE', #6474, #3890, #612, .T. ) ;
#2155 = CARTESIAN_POINT ( 'NONE',  ( 2.624999999999998668, -29.77083333265053611, -4.546633369868303021 ) ) ;
#2156 = CYLINDRICAL_SURFACE ( 'NONE', #4658, 1.500000000000000222 ) ;
#2157 = CARTESIAN_POINT ( 'NONE',  ( 9.180150650966086169E-15, -28.56249999999999645, 5.250000000000000000 ) ) ;
#2158 = CARTESIAN_POINT ( 'NONE',  ( 3.492485675378536047, -7.349340926099362292, 1.467888652719046672 ) ) ;
#2159 = CARTESIAN_POINT ( 'NONE',  ( 0.01814118441321408565, -7.849340926099360516, -3.500000000000000000 ) ) ;
#2160 = ORIENTED_EDGE ( 'NONE', *, *, #6275, .F. ) ;
#2161 = CARTESIAN_POINT ( 'NONE',  ( 1.406733260263385521, -29.17633545031537423, 5.250000000000006217 ) ) ;
#2162 = CARTESIAN_POINT ( 'NONE',  ( -5.250000000000000000, -26.92708333401612819, -3.031088913245536531 ) ) ;
#2163 = ORIENTED_EDGE ( 'NONE', *, *, #7789, .T. ) ;
#2164 = VERTEX_POINT ( 'NONE', #507 ) ;
#2165 = CYLINDRICAL_SURFACE ( 'NONE', #7932, 5.250000000000000000 ) ;
#2166 = CARTESIAN_POINT ( 'NONE',  ( -3.500000000000000000, -4.550659073900638951, 0.01814118441314012051 ) ) ;
#2167 = DIRECTION ( 'NONE',  ( 0.000000000000000000, 0.000000000000000000, -1.000000000000000000 ) ) ;
#2168 = VERTEX_POINT ( 'NONE', #8369 ) ;
#2169 = CARTESIAN_POINT ( 'NONE',  ( -9.180150650966086169E-15, -28.37499999931720041, 5.249999999999999112 ) ) ;
#2170 = CYLINDRICAL_SURFACE ( 'NONE', #2847, 1.749999999999999778 ) ;
#2171 = CARTESIAN_POINT ( 'NONE',  ( 2.624999999999998668, -28.83333333333333215, -4.546633369868303021 ) ) ;
#2172 = CARTESIAN_POINT ( 'NONE',  ( 2.557341765624996821, -28.15104166700806587, 4.429445870380401828 ) ) ;
#2173 = FACE_OUTER_BOUND ( 'NONE', #8068, .T. ) ;
#2174 = MANIFOLD_SOLID_BREP ( 'Boss-Extrude3', #3869 ) ;
#2175 = CARTESIAN_POINT ( 'NONE',  ( -2.625000000000002220, -28.86458333401612819, 4.546633369868302132 ) ) ;
#2176 = CARTESIAN_POINT ( 'NONE',  ( -1.224499502706077880, -3.149340926099362115, -3.007514324621463064 ) ) ;
#2177 = CARTESIAN_POINT ( 'NONE',  ( 0.000000000000000000, -29.00000000000000355, 0.000000000000000000 ) ) ;
#2178 = CARTESIAN_POINT ( 'NONE',  ( 5.385316468749999252, -28.21354166632526983, -3.109213912904139399 ) ) ;
#2179 = CARTESIAN_POINT ( 'NONE',  ( -2.815599370228907272, -6.350659073900638774, 2.841254879263473754 ) ) ;
#2180 = CARTESIAN_POINT ( 'NONE',  ( 5.249999999999999112, -27.22916666666666430, -3.031088913245534755 ) ) ;
#2181 = CARTESIAN_POINT ( 'NONE',  ( 0.000000000000000000, -30.00000000000000000, 5.250000000000000000 ) ) ;
#2182 = ADVANCED_FACE ( 'NONE', ( #6075, #4090 ), #7668, .T. ) ;
#2183 = EDGE_LOOP ( 'NONE', ( #7881, #4303, #254 ) ) ;
#2184 = CARTESIAN_POINT ( 'NONE',  ( 5.250000000000000888, -29.89583333333333215, 3.031088913245532979 ) ) ;
#2185 = ORIENTED_EDGE ( 'NONE', *, *, #5655, .T. ) ;
#2186 = DIRECTION ( 'NONE',  ( 0.000000000000000000, 0.000000000000000000, 1.000000000000000000 ) ) ;
#2187 = CARTESIAN_POINT ( 'NONE',  ( 3.007514324621436863, -2.050659073900639839, 1.224499502706140719 ) ) ;
#2188 = ORIENTED_EDGE ( 'NONE', *, *, #1496, .F. ) ;
#2189 = CARTESIAN_POINT ( 'NONE',  ( 2.625000000000000444, -29.70833333333333215, -4.546633369868303021 ) ) ;
#2190 = FACE_OUTER_BOUND ( 'NONE', #1371, .T. ) ;
#2191 = PRODUCT_DEFINITION_FORMATION_WITH_SPECIFIED_SOURCE ( 'ANY', '', #4156, .NOT_KNOWN. ) ;
#2192 = CARTESIAN_POINT ( 'NONE',  ( 2.557341765624996821, -27.46354166700806587, 4.429445870380401828 ) ) ;
#2193 = EDGE_CURVE ( 'NONE', #8808, #3057, #763, .T. ) ;
#2194 = SURFACE_SIDE_STYLE ('',( #8483 ) ) ;
#2195 = CARTESIAN_POINT ( 'NONE',  ( 5.114683531249999859, -27.65104166700806232, -2.952963913586932776 ) ) ;
#2196 = DIRECTION ( 'NONE',  ( 0.000000000000000000, 1.000000000000000000, 0.000000000000000000 ) ) ;
#2197 = DIRECTION ( 'NONE',  ( 0.000000000000000000, -0.000000000000000000, -1.000000000000000000 ) ) ;
#2198 = CARTESIAN_POINT ( 'NONE',  ( 0.000000000000000000, -29.00000000000000355, 0.000000000000000000 ) ) ;
#2199 = CARTESIAN_POINT ( 'NONE',  ( 0.000000000000000000, -30.00000000000000000, 0.000000000000000000 ) ) ;
#2200 = CARTESIAN_POINT ( 'NONE',  ( 5.114683531249999859, -29.65104166700806232, -2.952963913586932776 ) ) ;
#2201 = CARTESIAN_POINT ( 'NONE',  ( 3.500000000000000000, -5.849340926099361404, 0.01814118441321387054 ) ) ;
#2202 = VERTEX_POINT ( 'NONE', #4732 ) ;
#2203 = CARTESIAN_POINT ( 'NONE',  ( -3.500000000000000000, 0.2493409260993610654, 0.01814118441314012051 ) ) ;
#2204 = CARTESIAN_POINT ( 'NONE',  ( 5.250000000000000000, -27.99999999999999645, 0.000000000000000000 ) ) ;
#2205 = CARTESIAN_POINT ( 'NONE',  ( -5.114683531250000748, -27.96354166700806587, 2.952963913586931888 ) ) ;
#2206 = EDGE_LOOP ( 'NONE', ( #5156, #2359, #139 ) ) ;
#2207 = ORIENTED_EDGE ( 'NONE', *, *, #6586, .F. ) ;
#2208 = DIRECTION ( 'NONE',  ( 0.000000000000000000, 0.000000000000000000, 1.000000000000000000 ) ) ;
#2209 = CARTESIAN_POINT ( 'NONE',  ( 2.692658234375002735, -27.27604166632526628, 4.663820869356205101 ) ) ;
#2210 = CARTESIAN_POINT ( 'NONE',  ( -1.674995433905516196, -1.050659073900638507, -3.992485675378566690 ) ) ;
#2211 = CARTESIAN_POINT ( 'NONE',  ( 0.000000000000000000, -20.00000000000000000, -1.499999999999999778 ) ) ;
#2212 = VERTEX_POINT ( 'NONE', #1204 ) ;
#2213 = CARTESIAN_POINT ( 'NONE',  ( -5.250000000000000000, -27.62500000000000000, -6.429395695523604153E-16 ) ) ;
#2214 = DIRECTION ( 'NONE',  ( 1.000000000000000000, 0.000000000000000000, 0.000000000000000000 ) ) ;
#2215 = FACE_OUTER_BOUND ( 'NONE', #6032, .T. ) ;
#2216 = AXIS2_PLACEMENT_3D ( 'NONE', #3437, #6390, #7094 ) ;
#2217 = CARTESIAN_POINT ( 'NONE',  ( -5.114683531250000748, -27.73437500034139802, -6.263680815196995234E-16 ) ) ;
#2218 = CARTESIAN_POINT ( 'NONE',  ( 0.000000000000000000, -27.00000000000000000, 0.000000000000000000 ) ) ;
#2219 = CARTESIAN_POINT ( 'NONE',  ( 0.000000000000000000, 74.00000000000001421, 2.500000000000000000 ) ) ;
#2220 = CARTESIAN_POINT ( 'NONE',  ( -3.007514324621463508, -6.749340926099361759, 1.224499502706077658 ) ) ;
#2221 = DIRECTION ( 'NONE',  ( -0.000000000000000000, -0.000000000000000000, 1.000000000000000000 ) ) ;
#2222 = CARTESIAN_POINT ( 'NONE',  ( -2.692658234375000514, -28.65104166632526628, -4.663820869356205989 ) ) ;
#2223 = EDGE_CURVE ( 'NONE', #8584, #6343, #2555, .T. ) ;
#2224 = CARTESIAN_POINT ( 'NONE',  ( -4.007514324621467949, -0.3493409260993607379, 1.638713065079161924 ) ) ;
#2225 = CIRCLE ( 'NONE', #7429, 2.750000000000000000 ) ;
#2226 = CARTESIAN_POINT ( 'NONE',  ( 0.000000000000000000, -9.000000000000001776, 5.250000000000000000 ) ) ;
#2227 = CARTESIAN_POINT ( 'NONE',  ( -5.250000000000000000, -26.90625000068279604, -6.429395695523604153E-16 ) ) ;
#2228 = CIRCLE ( 'NONE', #3431, 2.629341307491595447 ) ;
#2229 = DIRECTION ( 'NONE',  ( 0.000000000000000000, 0.000000000000000000, 1.000000000000000000 ) ) ;
#2230 = ORIENTED_EDGE ( 'NONE', *, *, #6137, .T. ) ;
#2231 = CARTESIAN_POINT ( 'NONE',  ( -2.692658234375000514, -27.11979166632526628, -4.663820869356205989 ) ) ;
#2232 = ORIENTED_EDGE ( 'NONE', *, *, #9006, .T. ) ;
#2233 = CARTESIAN_POINT ( 'NONE',  ( -3.807688866302469071E-16, -27.14062499965860198, -6.218427825808274356 ) ) ;
#2234 = CARTESIAN_POINT ( 'NONE',  ( -2.992485675378564469, -4.650659073900640372, 1.260781871532430820 ) ) ;
#2235 = VECTOR ( 'NONE', #6110, 1000.000000000000000 ) ;
#2236 = ORIENTED_EDGE ( 'NONE', *, *, #5626, .F. ) ;
#2237 = CARTESIAN_POINT ( 'NONE',  ( -1.113604000661152470E-15, -29.06250000000000000, 6.062177826491070398 ) ) ;
#2238 = DIRECTION ( 'NONE',  ( -0.000000000000000000, 1.000000000000000000, -0.000000000000000000 ) ) ;
#2239 =( BOUNDED_CURVE ( )  B_SPLINE_CURVE ( 2, ( #727, #2886, #1427, #683, #6948, #8547, #2175, #9148, #4955 ),
 .UNSPECIFIED., .F., .F. ) 
 B_SPLINE_CURVE_WITH_KNOTS ( ( 3, 2, 2, 2, 3 ),
 ( 0.2708333333333333148, 0.2777777777777777901, 0.2916666666666666852, 0.3055555555555555802, 0.3125000000000000000 ),
 .UNSPECIFIED. ) 
 CURVE ( )  GEOMETRIC_REPRESENTATION_ITEM ( )  RATIONAL_B_SPLINE_CURVE ( ( 0.9330127018922194093, 0.9330127018922190762, 1.000000000000000000, 0.8660254037844387076, 1.000000000000000000, 0.8660254037844387076, 1.000000000000000000, 0.9330127018922194093, 0.9330127018922194093 ) ) 
 REPRESENTATION_ITEM ( '' )  );
#2240 = CARTESIAN_POINT ( 'NONE',  ( -5.114683531250000748, -27.29687500034139802, -6.263680815196995234E-16 ) ) ;
#2241 = VECTOR ( 'NONE', #72, 1000.000000000000000 ) ;
#2242 = FILL_AREA_STYLE ('',( #8565 ) ) ;
#2243 = CARTESIAN_POINT ( 'NONE',  ( -5.114683531250000748, -28.04687500034139802, -6.263680815196995234E-16 ) ) ;
#2244 = CARTESIAN_POINT ( 'NONE',  ( -3.492485675378536047, -1.749340926099361093, -1.467888652719048670 ) ) ;
#2245 = CARTESIAN_POINT ( 'NONE',  ( -2.625000000000000444, -29.97916666598387181, -4.546633369868303021 ) ) ;
#2246 = CARTESIAN_POINT ( 'NONE',  ( -5.249999999999997335, -28.22916666666666430, 3.031088913245538308 ) ) ;
#2247 = CARTESIAN_POINT ( 'NONE',  ( -1.084901341431563923E-15, -29.48437500034139802, 5.905927827173866440 ) ) ;
#2248 = CARTESIAN_POINT ( 'NONE',  ( -0.01814118441321365544, -5.449340926099361937, 3.500000000000000000 ) ) ;
#2249 = VERTEX_POINT ( 'NONE', #9007 ) ;
#2250 = DIRECTION ( 'NONE',  ( 0.000000000000000000, -1.000000000000000000, 0.000000000000000000 ) ) ;
#2251 = DIRECTION ( 'NONE',  ( 0.000000000000000000, 0.000000000000000000, 1.000000000000000000 ) ) ;
#2252 = CARTESIAN_POINT ( 'NONE',  ( -1.084901341431563923E-15, -27.92187500034139802, 5.905927827173866440 ) ) ;
#2253 = EDGE_CURVE ( 'NONE', #8014, #3220, #5474, .T. ) ;
#2254 = ORIENTED_EDGE ( 'NONE', *, *, #7167, .F. ) ;
#2255 = ORIENTED_EDGE ( 'NONE', *, *, #4966, .F. ) ;
#2256 = LINE ( 'NONE', #3700, #3036 ) ;
#2257 = CARTESIAN_POINT ( 'NONE',  ( -2.692658234375000514, -27.90104166632526628, -4.663820869356205989 ) ) ;
#2258 = CARTESIAN_POINT ( 'NONE',  ( -2.841254879263533262, -0.4493409260993607157, 2.815599370228847764 ) ) ;
#2259 =( NAMED_UNIT ( * ) SI_UNIT ( $, .STERADIAN. ) SOLID_ANGLE_UNIT ( ) );
#2260 = VERTEX_POINT ( 'NONE', #8456 ) ;
#2261 = PLANE ( 'NONE',  #7002 ) ;
#2262 = CARTESIAN_POINT ( 'NONE',  ( 3.712013335537174572E-16, -29.46875000068279604, -6.062177826491070398 ) ) ;
#2263 = CARTESIAN_POINT ( 'NONE',  ( 5.385316468750001029, -28.50520833299193058, 3.109213912904135846 ) ) ;
#2264 = UNCERTAINTY_MEASURE_WITH_UNIT (LENGTH_MEASURE( 1.000000000000000082E-05 ), #1781, 'distance_accuracy_value', 'NONE');
#2265 = CARTESIAN_POINT ( 'NONE',  ( -5.114683531249999859, -27.25520833367473017, -2.952963913586935440 ) ) ;
#2266 = CARTESIAN_POINT ( 'NONE',  ( 3.500000000000000000, -2.649340926099361226, 0.01814118441321387054 ) ) ;
#2267 = CARTESIAN_POINT ( 'NONE',  ( 5.249999999999999112, -28.79166666598386826, -3.031088913245536975 ) ) ;
#2268 = CARTESIAN_POINT ( 'NONE',  ( 3.007514324621436863, -3.650659073900639928, 1.224499502706140719 ) ) ;
#2269 = CARTESIAN_POINT ( 'NONE',  ( -2.033577675846918216E-14, -29.37499999931720396, 5.250000000000000888 ) ) ;
#2270 = CARTESIAN_POINT ( 'NONE',  ( -0.01814118441321889430, -2.249340926099360427, 4.000000000000000000 ) ) ;
#2271 = AXIS2_PLACEMENT_3D ( 'NONE', #198, #4065, #1086 ) ;
#2272 = CARTESIAN_POINT ( 'NONE',  ( 5.250000000000000000, -28.31249999931720396, -6.429395695523604153E-16 ) ) ;
#2273 = DIRECTION ( 'NONE',  ( -0.000000000000000000, -1.000000000000000000, -0.000000000000000000 ) ) ;
#2274 = CARTESIAN_POINT ( 'NONE',  ( 3.061616997868383141E-16, 79.00000000000001421, -2.500000000000000000 ) ) ;
#2275 = CARTESIAN_POINT ( 'NONE',  ( 5.250000000000000888, -29.83333333265053611, 3.031088913245533423 ) ) ;
#2276 = ORIENTED_EDGE ( 'NONE', *, *, #7313, .F. ) ;
#2277 = CIRCLE ( 'NONE', #2586, 4.199909308207394609 ) ;
#2278 = DIRECTION ( 'NONE',  ( 1.000000000000000000, 0.000000000000000000, 0.000000000000000000 ) ) ;
#2279 = CARTESIAN_POINT ( 'NONE',  ( 5.385316468749999252, -28.43229166632526983, -3.109213912904139399 ) ) ;
#2280 = CARTESIAN_POINT ( 'NONE',  ( 2.161402558328724325E-14, -28.81250000000000355, -5.250000000000000000 ) ) ;
#2281 = ORIENTED_EDGE ( 'NONE', *, *, #1000, .T. ) ;
#2282 = CARTESIAN_POINT ( 'NONE',  ( -2.625000000000000444, -27.29166666666666430, -4.546633369868303021 ) ) ;
#2283 = CARTESIAN_POINT ( 'NONE',  ( 3.000000000000000444, -5.350659073900639662, -0.01814118441314496039 ) ) ;
#2284 = ORIENTED_EDGE ( 'NONE', *, *, #6586, .T. ) ;
#2285 = CARTESIAN_POINT ( 'NONE',  ( 5.250000000000000000, -29.75000000000000000, 0.000000000000000000 ) ) ;
#2286 = CIRCLE ( 'NONE', #6736, 6.250000000000000000 ) ;
#2287 = CARTESIAN_POINT ( 'NONE',  ( -1.084901341431563726E-15, -27.48437500034139802, 5.905927827173866440 ) ) ;
#2288 =( NAMED_UNIT ( * ) PLANE_ANGLE_UNIT ( ) SI_UNIT ( $, .RADIAN. ) );
#2289 = CARTESIAN_POINT ( 'NONE',  ( -5.114683531250000748, -27.29687500034139802, -6.263680815196995234E-16 ) ) ;
#2290 = CARTESIAN_POINT ( 'NONE',  ( 0.000000000000000000, -30.00000000000000000, 0.000000000000000000 ) ) ;
#2291 =( BOUNDED_CURVE ( )  B_SPLINE_CURVE ( 2, ( #4540, #7372, #8768, #5131, #7327, #812, #252, #7938, #1559 ),
 .UNSPECIFIED., .F., .F. ) 
 B_SPLINE_CURVE_WITH_KNOTS ( ( 3, 2, 2, 2, 3 ),
 ( 0.6875000000000000000, 0.6944444444444444198, 0.7083333333333333703, 0.7222222222222222099, 0.7291666666666667407 ),
 .UNSPECIFIED. ) 
 CURVE ( )  GEOMETRIC_REPRESENTATION_ITEM ( )  RATIONAL_B_SPLINE_CURVE ( ( 0.9330127018922194093, 0.9330127018922194093, 1.000000000000000000, 0.8660254037844387076, 1.000000000000000000, 0.8660254037844387076, 1.000000000000000000, 0.9330127018922187432, 0.9330127018922192983 ) ) 
 REPRESENTATION_ITEM ( '' )  );
#2292 = CARTESIAN_POINT ( 'NONE',  ( 0.01814118441321408565, -6.249340926099360871, -3.500000000000000000 ) ) ;
#2293 = PLANE ( 'NONE',  #4015 ) ;
#2294 = CARTESIAN_POINT ( 'NONE',  ( -6.972266317189433020E-16, -28.31249999999999645, -5.250000000000000000 ) ) ;
#2295 = CARTESIAN_POINT ( 'NONE',  ( 2.557341765625000818, -29.88020833367473372, -4.429445870380400052 ) ) ;
#2296 = FILL_AREA_STYLE_COLOUR ( '', #787 ) ;
#2297 = EDGE_CURVE ( 'NONE', #7186, #8226, #1334, .T. ) ;
#2298 = EDGE_LOOP ( 'NONE', ( #5873, #4439, #7699, #7334 ) ) ;
#2299 = CARTESIAN_POINT ( 'NONE',  ( 0.01814118441313990887, -6.550659073900639839, 3.500000000000000000 ) ) ;
#2300 = PLANE ( 'NONE',  #4310 ) ;
#2301 = CARTESIAN_POINT ( 'NONE',  ( 3.616337804771879580E-16, -29.04687500034139802, -5.905927827173866440 ) ) ;
#2302 =( REPRESENTATION_RELATIONSHIP ('NONE','NONE', #735, #3797 ) REPRESENTATION_RELATIONSHIP_WITH_TRANSFORMATION ( #7103 )SHAPE_REPRESENTATION_RELATIONSHIP( ) );
#2303 = ORIENTED_EDGE ( 'NONE', *, *, #1165, .F. ) ;
#2304 = EDGE_CURVE ( 'NONE', #6523, #3606, #2746, .T. ) ;
#2305 = CARTESIAN_POINT ( 'NONE',  ( 0.000000000000000000, -30.00000000000000000, 0.000000000000000000 ) ) ;
#2306 = CARTESIAN_POINT ( 'NONE',  ( 5.385316468750000141, -27.73437499965860198, -6.595110575850215044E-16 ) ) ;
#2307 = CARTESIAN_POINT ( 'NONE',  ( -2.841254879263473310, -4.350659073900638774, -2.815599370228907716 ) ) ;
#2308 = CARTESIAN_POINT ( 'NONE',  ( -5.250000000000000888, -29.10416666666666785, 3.031088913245533423 ) ) ;
#2309 = ORIENTED_EDGE ( 'NONE', *, *, #5158, .T. ) ;
#2310 = DIRECTION ( 'NONE',  ( 0.000000000000000000, 1.000000000000000000, 0.000000000000000000 ) ) ;
#2311 = LINE ( 'NONE', #165, #6391 ) ;
#2312 = CARTESIAN_POINT ( 'NONE',  ( -2.692658234375000514, -28.40104166632526628, -4.663820869356205989 ) ) ;
#2313 = CARTESIAN_POINT ( 'NONE',  ( 2.557341765624996821, -27.90104166700806587, 4.429445870380401828 ) ) ;
#2314 = CARTESIAN_POINT ( 'NONE',  ( -1.467888652719046449, -0.5493409260993611376, 3.492485675378536047 ) ) ;
#2315 = CARTESIAN_POINT ( 'NONE',  ( -5.385316468749998364, -27.30729166632526272, 3.109213912904140287 ) ) ;
#2316 = CARTESIAN_POINT ( 'NONE',  ( 3.000000000000000444, -3.750659073900639573, -0.01814118441314496039 ) ) ;
#2317 = CARTESIAN_POINT ( 'NONE',  ( 0.000000000000000000, -27.00000000000000000, 0.000000000000000000 ) ) ;
#2318 = CARTESIAN_POINT ( 'NONE',  ( 4.000000000000000000, -6.950659073900639306, -0.01814118441313441674 ) ) ;
#2319 = CARTESIAN_POINT ( 'NONE',  ( 1.113604000661152470E-15, -28.12499999931720041, 6.062177826491070398 ) ) ;
#2320 = CARTESIAN_POINT ( 'NONE',  ( 2.625000000000002220, -27.66666666666666430, 4.546633369868302132 ) ) ;
#2321 = CARTESIAN_POINT ( 'NONE',  ( -1.000000000000000000, -35.00000000000000000, 1.118033988749894458 ) ) ;
#2322 = DIRECTION ( 'NONE',  ( 0.000000000000000000, 1.000000000000000000, 0.000000000000000000 ) ) ;
#2323 = ORIENTED_EDGE ( 'NONE', *, *, #8402, .T. ) ;
#2324 = CARTESIAN_POINT ( 'NONE',  ( -5.385316468750001029, -28.34895833299193058, -3.109213912904136734 ) ) ;
#2325 = EDGE_CURVE ( 'NONE', #8116, #4614, #3674, .T. ) ;
#2326 = CARTESIAN_POINT ( 'NONE',  ( -2.841254879263533262, -5.249340926099361759, 2.815599370228847764 ) ) ;
#2327 = DIRECTION ( 'NONE',  ( 0.000000000000000000, -1.000000000000000000, 0.000000000000000000 ) ) ;
#2328 = ORIENTED_EDGE ( 'NONE', *, *, #6043, .F. ) ;
#2329 = CARTESIAN_POINT ( 'NONE',  ( 5.114683531250000748, -26.85937500034139802, 0.000000000000000000 ) ) ;
#2330 = CARTESIAN_POINT ( 'NONE',  ( 0.01814118441313990887, -0.1506590739006389568, 3.500000000000000000 ) ) ;
#2331 = VERTEX_POINT ( 'NONE', #8412 ) ;
#2332 = CARTESIAN_POINT ( 'NONE',  ( -5.250000000000000000, -27.39583333333332860, -3.031088913245536531 ) ) ;
#2333 = CARTESIAN_POINT ( 'NONE',  ( -1.084901341431563726E-15, -27.98437500034139802, 5.905927827173866440 ) ) ;
#2334 = CARTESIAN_POINT ( 'NONE',  ( 0.000000000000000000, -20.00000000000000000, -1.500000000000000222 ) ) ;
#2335 = CARTESIAN_POINT ( 'NONE',  ( 2.625000000000002220, -30.10416666598386826, 4.546633369868302132 ) ) ;
#2336 = CARTESIAN_POINT ( 'NONE',  ( 3.500000000000000000, -4.249340926099360871, 0.01814118441321387054 ) ) ;
#2337 = CARTESIAN_POINT ( 'NONE',  ( -5.249999999999997335, -29.91666666598387181, 3.031088913245538308 ) ) ;
#2338 = CARTESIAN_POINT ( 'NONE',  ( 6.972266317189433020E-16, -28.68749999999999645, -5.250000000000000000 ) ) ;
#2339 = DIRECTION ( 'NONE',  ( 1.000000000000000000, 0.000000000000000000, 0.000000000000000000 ) ) ;
#2340 = STYLED_ITEM ( 'NONE', ( #3137 ), #4954 ) ;
#2341 = FILL_AREA_STYLE ('',( #2296 ) ) ;
#2342 = ORIENTED_EDGE ( 'NONE', *, *, #3349, .T. ) ;
#2343 = DIRECTION ( 'NONE',  ( 1.044949058366721163E-14, 0.07256473765270718412, -0.9973637043974449279 ) ) ;
#2344 = CARTESIAN_POINT ( 'NONE',  ( 2.624999999999996891, -28.04166666666666785, 4.546633369868304797 ) ) ;
#2345 = CARTESIAN_POINT ( 'NONE',  ( -2.557341765625002594, -27.94270833367473017, 4.429445870380399164 ) ) ;
#2346 =( BOUNDED_CURVE ( )  B_SPLINE_CURVE ( 2, ( #3197, #6018, #393, #1797, #4767 ),
 .UNSPECIFIED., .F., .F. ) 
 B_SPLINE_CURVE_WITH_KNOTS ( ( 3, 2, 3 ),
 ( 0.000000000000000000, 0.01388888888888888812, 0.02083333333333333218 ),
 .UNSPECIFIED. ) 
 CURVE ( )  GEOMETRIC_REPRESENTATION_ITEM ( )  RATIONAL_B_SPLINE_CURVE ( ( 1.000000000000000000, 0.8660254037844387076, 1.000000000000000000, 0.9330127018922194093, 0.9330127018922194093 ) ) 
 REPRESENTATION_ITEM ( '' )  );
#2347 = ORIENTED_EDGE ( 'NONE', *, *, #2994, .T. ) ;
#2348 = CARTESIAN_POINT ( 'NONE',  ( 2.033577675846918216E-14, -26.84375000068279959, 5.250000000000000888 ) ) ;
#2349 = CARTESIAN_POINT ( 'NONE',  ( -5.385316468749998364, -28.08854166632526628, 3.109213912904140287 ) ) ;
#2350 = CARTESIAN_POINT ( 'NONE',  ( -4.000000000000000000, -2.950659073900638862, 0.01814118441313491634 ) ) ;
#2351 = DIRECTION ( 'NONE',  ( 0.000000000000000000, -1.000000000000000000, 0.000000000000000000 ) ) ;
#2352 = ORIENTED_EDGE ( 'NONE', *, *, #4698, .T. ) ;
#2353 = CARTESIAN_POINT ( 'NONE',  ( 5.249999999999997335, -27.27083333333332860, 3.031088913245538308 ) ) ;
#2354 = EDGE_CURVE ( 'NONE', #4014, #7159, #2739, .T. ) ;
#2355 = CARTESIAN_POINT ( 'NONE',  ( 1.836970198721029688E-16, -20.00000000000000000, 1.499999999999999778 ) ) ;
#2356 = CARTESIAN_POINT ( 'NONE',  ( -2.625000000000002220, -29.11458333401613174, 4.546633369868302132 ) ) ;
#2357 = CARTESIAN_POINT ( 'NONE',  ( -5.385316468750000141, -28.10937499965860198, 0.000000000000000000 ) ) ;
#2358 = CARTESIAN_POINT ( 'NONE',  ( -2.557341765625002594, -29.75520833367473017, 4.429445870380399164 ) ) ;
#2359 = ORIENTED_EDGE ( 'NONE', *, *, #885, .F. ) ;
#2360 = CIRCLE ( 'NONE', #3409, 1.500000000000000222 ) ;
#2361 = CARTESIAN_POINT ( 'NONE',  ( 0.000000000000000000, -46.00000000000000000, 0.000000000000000000 ) ) ;
#2362 = CARTESIAN_POINT ( 'NONE',  ( -1.260781871532431708, -4.250659073900640017, -2.992485675378564469 ) ) ;
#2363 = DIRECTION ( 'NONE',  ( 0.000000000000000000, 1.000000000000000000, 0.000000000000000000 ) ) ;
#2364 = CARTESIAN_POINT ( 'NONE',  ( 2.841254879263533262, -1.249340926099360871, -2.815599370228847320 ) ) ;
#2365 = EDGE_CURVE ( 'NONE', #179, #8145, #3524, .T. ) ;
#2366 = CARTESIAN_POINT ( 'NONE',  ( -5.250000000000000000, -27.43749999931720396, 0.000000000000000000 ) ) ;
#2367 = DIRECTION ( 'NONE',  ( 1.067350013832299517E-17, -0.9961946980917455452, 0.08715574274765836016 ) ) ;
#2368 = CARTESIAN_POINT ( 'NONE',  ( -3.507514324621464397, -1.949340926099361271, 1.431606283892619569 ) ) ;
#2369 = EDGE_CURVE ( 'NONE', #3636, #4653, #5653, .T. ) ;
#2370 = DIRECTION ( 'NONE',  ( 1.000000000000000000, 0.000000000000000000, 0.000000000000000000 ) ) ;
#2371 = DIRECTION ( 'NONE',  ( 0.000000000000000000, 0.000000000000000000, 1.000000000000000000 ) ) ;
#2372 =( BOUNDED_CURVE ( )  B_SPLINE_CURVE ( 2, ( #5337, #363, #8187, #4647, #6782, #7488, #6640, #3122, #3955 ),
 .UNSPECIFIED., .F., .T. ) 
 B_SPLINE_CURVE_WITH_KNOTS ( ( 3, 2, 2, 2, 3 ),
 ( 0.7291666666666667407, 0.7361111111111111605, 0.7500000000000000000, 0.7638888888888888395, 0.7708333333333332593 ),
 .UNSPECIFIED. ) 
 CURVE ( )  GEOMETRIC_REPRESENTATION_ITEM ( )  RATIONAL_B_SPLINE_CURVE ( ( 0.9330127018922192983, 0.9330127018922198534, 1.000000000000000000, 0.8660254037844387076, 1.000000000000000000, 0.8660254037844387076, 1.000000000000000000, 0.9330127018922198534, 0.9330127018922192983 ) ) 
 REPRESENTATION_ITEM ( '' )  );
#2373 = CARTESIAN_POINT ( 'NONE',  ( -2.692658234375000514, -27.86979166632526628, -4.663820869356205989 ) ) ;
#2374 = CARTESIAN_POINT ( 'NONE',  ( -2.841254879263533262, -3.649340926099360782, 2.815599370228847764 ) ) ;
#2375 = DIRECTION ( 'NONE',  ( 0.000000000000000000, 0.000000000000000000, -1.000000000000000000 ) ) ;
#2376 = EDGE_LOOP ( 'NONE', ( #3934, #6046, #8764, #5352 ) ) ;
#2377 = CARTESIAN_POINT ( 'NONE',  ( 1.142306659890740623E-15, -28.51562499965860198, 6.218427825808274356 ) ) ;
#2378 = CARTESIAN_POINT ( 'NONE',  ( -3.007514324621435531, -7.650659073900639484, -1.224499502706142273 ) ) ;
#2379 = EDGE_LOOP ( 'NONE', ( #3605, #5087, #281, #6152 ) ) ;
#2380 = CARTESIAN_POINT ( 'NONE',  ( 3.712013335537174572E-16, -27.18750000000000000, -6.062177826491070398 ) ) ;
#2381 = AXIS2_PLACEMENT_3D ( 'NONE', #8404, #6381, #1986 ) ;
#2382 = CARTESIAN_POINT ( 'NONE',  ( 5.114683531250000748, -28.15104166700806587, -2.952963913586932776 ) ) ;
#2383 = CARTESIAN_POINT ( 'NONE',  ( 2.624999999999998668, -27.58333333333333570, -4.546633369868303021 ) ) ;
#2384 = CIRCLE ( 'NONE', #1637, 1.499999999999999778 ) ;
#2385 = CARTESIAN_POINT ( 'NONE',  ( -5.114683531250000748, -29.73437500034139802, -6.263680815196995234E-16 ) ) ;
#2386 = CARTESIAN_POINT ( 'NONE',  ( 3.492485675378536047, -2.549340926099360694, 1.467888652719046672 ) ) ;
#2387 = CARTESIAN_POINT ( 'NONE',  ( 5.114683531250000748, -29.89062500034139802, 0.000000000000000000 ) ) ;
#2388 = CARTESIAN_POINT ( 'NONE',  ( 5.250000000000000000, -28.74999999999999645, 0.000000000000000000 ) ) ;
#2389 = CARTESIAN_POINT ( 'NONE',  ( 3.616337804771879580E-16, -29.10937500034139447, -5.905927827173866440 ) ) ;
#2390 = CARTESIAN_POINT ( 'NONE',  ( 1.406733260263397289, -28.33258545099817027, 5.249999999999997335 ) ) ;
#2391 = ORIENTED_EDGE ( 'NONE', *, *, #1915, .T. ) ;
#2392 = CARTESIAN_POINT ( 'NONE',  ( 0.000000000000000000, 73.00000000000001421, -4.000000000000000000 ) ) ;
#2393 = AXIS2_PLACEMENT_3D ( 'NONE', #4264, #5741, #6395 ) ;
#2394 = CARTESIAN_POINT ( 'NONE',  ( -5.114683531250000748, -28.71354166700806587, 2.952963913586931888 ) ) ;
#2395 = ORIENTED_EDGE ( 'NONE', *, *, #4371, .T. ) ;
#2396 = DIRECTION ( 'NONE',  ( 0.000000000000000000, 1.000000000000000000, 0.000000000000000000 ) ) ;
#2397 = CARTESIAN_POINT ( 'NONE',  ( -5.385316468749998364, -27.33854166632526628, 3.109213912904140287 ) ) ;
#2398 = CARTESIAN_POINT ( 'NONE',  ( 1.674995433905515085, -6.650659073900639484, 3.992485675378568022 ) ) ;
#2399 = UNCERTAINTY_MEASURE_WITH_UNIT (LENGTH_MEASURE( 1.000000000000000082E-05 ), #4022, 'distance_accuracy_value', 'NONE');
#2400 = CARTESIAN_POINT ( 'NONE',  ( -2.692658234375000514, -27.40104166632526628, -4.663820869356205989 ) ) ;
#2401 = ORIENTED_EDGE ( 'NONE', *, *, #8673, .F. ) ;
#2402 = CARTESIAN_POINT ( 'NONE',  ( -6.972266317189433020E-16, -28.49999999931720041, -5.249999999999999112 ) ) ;
#2403 = CARTESIAN_POINT ( 'NONE',  ( -5.250000000000000000, -29.17708333401612819, -3.031088913245536531 ) ) ;
#2404 = CARTESIAN_POINT ( 'NONE',  ( 5.385316468750001029, -28.25520833299193413, 3.109213912904135846 ) ) ;
#2405 = CARTESIAN_POINT ( 'NONE',  ( 2.557341765625000818, -27.06770833367473017, -4.429445870380400052 ) ) ;
#2406 = EDGE_LOOP ( 'NONE', ( #260, #3747, #8339, #5465 ) ) ;
#2407 = CARTESIAN_POINT ( 'NONE',  ( 5.385316468750001029, -27.22395833299193413, 3.109213912904134958 ) ) ;
#2408 = CARTESIAN_POINT ( 'NONE',  ( -1.224499502706140497, -3.250659073900639573, 3.007514324621436863 ) ) ;
#2409 = LINE ( 'NONE', #7337, #2824 ) ;
#2410 = EDGE_CURVE ( 'NONE', #977, #3365, #4358, .T. ) ;
#2411 = CARTESIAN_POINT ( 'NONE',  ( -3.712013335537174572E-16, -28.49999999931720396, -6.062177826491070398 ) ) ;
#2412 = CARTESIAN_POINT ( 'NONE',  ( 0.000000000000000000, -30.00000000000000000, 0.000000000000000000 ) ) ;
#2413 = CARTESIAN_POINT ( 'NONE',  ( -1.467888652719046449, -0.5493409260993611376, 3.492485675378535603 ) ) ;
#2414 = EDGE_CURVE ( 'NONE', #4395, #3979, #8542, .T. ) ;
#2415 = CARTESIAN_POINT ( 'NONE',  ( 5.250000000000000888, -29.58333333265053611, 3.031088913245533423 ) ) ;
#2416 = DIRECTION ( 'NONE',  ( 1.000000000000000000, 0.000000000000000000, 0.000000000000000000 ) ) ;
#2417 = CARTESIAN_POINT ( 'NONE',  ( 0.000000000000000000, 0.000000000000000000, 0.000000000000000000 ) ) ;
#2418 = CARTESIAN_POINT ( 'NONE',  ( -5.385316468750001029, -27.84895833299193413, -3.109213912904136734 ) ) ;
#2419 = CARTESIAN_POINT ( 'NONE',  ( 3.992485675378533383, -7.349340926099363180, 1.674995433905599462 ) ) ;
#2420 = CARTESIAN_POINT ( 'NONE',  ( 0.000000000000000000, -20.00000000000000000, -3.500000000000000444 ) ) ;
#2421 = ORIENTED_EDGE ( 'NONE', *, *, #5655, .F. ) ;
#2422 = CARTESIAN_POINT ( 'NONE',  ( 5.385316468750000141, -28.70312499965860198, -6.595110575850215044E-16 ) ) ;
#2423 = CARTESIAN_POINT ( 'NONE',  ( -1.431606283892693066, -0.05065907390063895815, 3.507514324621434199 ) ) ;
#2424 = VECTOR ( 'NONE', #9129, 1000.000000000000000 ) ;
#2425 = ORIENTED_EDGE ( 'NONE', *, *, #362, .T. ) ;
#2426 = CARTESIAN_POINT ( 'NONE',  ( -2.625000000000002220, -28.33333333333333215, 4.546633369868302132 ) ) ;
#2427 = APPLICATION_CONTEXT ( 'automotive_design' ) ;
#2428 = EDGE_CURVE ( 'NONE', #1704, #2936, #3714, .T. ) ;
#2429 = CARTESIAN_POINT ( 'NONE',  ( 5.114683531249998971, -26.94270833367473372, 2.952963913586936329 ) ) ;
#2430 = AXIS2_PLACEMENT_3D ( 'NONE', #6224, #8867, #5333 ) ;
#2431 = VERTEX_POINT ( 'NONE', #7805 ) ;
#2432 = SURFACE_SIDE_STYLE ('',( #8055 ) ) ;
#2433 = CARTESIAN_POINT ( 'NONE',  ( -5.250000000000000000, -27.77083333333333215, -3.031088913245534755 ) ) ;
#2434 = VERTEX_POINT ( 'NONE', #635 ) ;
#2435 = CARTESIAN_POINT ( 'NONE',  ( 3.616337804771879580E-16, -28.54687500034139802, -5.905927827173866440 ) ) ;
#2436 = CARTESIAN_POINT ( 'NONE',  ( 2.462045979635577364, -0.8493409260993610710, 2.487701488670255312 ) ) ;
#2437 = CARTESIAN_POINT ( 'NONE',  ( 5.114683531250000748, -26.92187500034139802, 0.000000000000000000 ) ) ;
#2438 = CARTESIAN_POINT ( 'NONE',  ( -2.624999999999996891, -27.70833333333333215, 4.546633369868304797 ) ) ;
#2439 = CARTESIAN_POINT ( 'NONE',  ( 2.557341765625000818, -29.38020833367473017, -4.429445870380400052 ) ) ;
#2440 = PLANE ( 'NONE',  #3474 ) ;
#2441 = AXIS2_PLACEMENT_3D ( 'NONE', #5660, #7852, #2043 ) ;
#2442 = ORIENTED_EDGE ( 'NONE', *, *, #1307, .T. ) ;
#2443 = DIRECTION ( 'NONE',  ( 0.000000000000000000, 1.000000000000000000, 0.000000000000000000 ) ) ;
#2444 = CARTESIAN_POINT ( 'NONE',  ( -5.114683531249999859, -27.25520833367473017, -2.952963913586935440 ) ) ;
#2445 = EDGE_CURVE ( 'NONE', #7820, #4395, #9183, .T. ) ;
#2446 = EDGE_LOOP ( 'NONE', ( #6124, #8578, #8790, #2452 ) ) ;
#2447 = FACE_OUTER_BOUND ( 'NONE', #4238, .T. ) ;
#2448 = CARTESIAN_POINT ( 'NONE',  ( 5.385316468750000141, -29.23437499965859843, -6.595110575850215044E-16 ) ) ;
#2449 = CARTESIAN_POINT ( 'NONE',  ( 1.638713065079247855, -7.250659073900640017, -4.007514324621431534 ) ) ;
#2450 = CARTESIAN_POINT ( 'NONE',  ( 2.300847884672513123E-14, -28.43750000000000000, -5.250000000000000000 ) ) ;
#2451 = CARTESIAN_POINT ( 'NONE',  ( 1.142306659890740623E-15, -27.54687499965860198, 6.218427825808274356 ) ) ;
#2452 = ORIENTED_EDGE ( 'NONE', *, *, #3497, .F. ) ;
#2453 = DIRECTION ( 'NONE',  ( 0.000000000000000000, 0.000000000000000000, 1.000000000000000000 ) ) ;
#2454 = CARTESIAN_POINT ( 'NONE',  ( 3.712013335537174572E-16, -29.71875000068279604, -6.062177826491070398 ) ) ;
#2455 = CARTESIAN_POINT ( 'NONE',  ( 5.385316468750000141, -28.48437499965860198, -6.595110575850215044E-16 ) ) ;
#2456 = UNCERTAINTY_MEASURE_WITH_UNIT (LENGTH_MEASURE( 1.000000000000000082E-05 ), #8517, 'distance_accuracy_value', 'NONE');
#2457 = ORIENTED_EDGE ( 'NONE', *, *, #8536, .T. ) ;
#2458 = DIRECTION ( 'NONE',  ( 0.000000000000000000, -0.000000000000000000, 1.000000000000000000 ) ) ;
#2459 = CARTESIAN_POINT ( 'NONE',  ( 2.992485675378565357, -0.6506590739006395951, -1.260781871532430376 ) ) ;
#2460 = DIRECTION ( 'NONE',  ( 1.000000000000000000, 0.000000000000000000, 0.000000000000000000 ) ) ;
#2461 = CARTESIAN_POINT ( 'NONE',  ( 1.113604000661152470E-15, -27.37499999931720041, 6.062177826491070398 ) ) ;
#2462 = CARTESIAN_POINT ( 'NONE',  ( -5.249999999999997335, -27.66666666598386826, 3.031088913245538308 ) ) ;
#2463 = CARTESIAN_POINT ( 'NONE',  ( -3.507514324621464397, -5.149340926099361226, 1.431606283892619569 ) ) ;
#2464 = DIRECTION ( 'NONE',  ( 0.000000000000000000, 0.000000000000000000, 1.000000000000000000 ) ) ;
#2465 = EDGE_LOOP ( 'NONE', ( #1482, #323, #2987, #1925 ) ) ;
#2466 = DIRECTION ( 'NONE',  ( 0.000000000000000000, 0.000000000000000000, 1.000000000000000000 ) ) ;
#2467 = CARTESIAN_POINT ( 'NONE',  ( 2.692658234374998738, -28.66145833299193413, -4.663820869356206877 ) ) ;
#2468 = CARTESIAN_POINT ( 'NONE',  ( -0.01814118441321889430, -3.849340926099360960, 4.000000000000000000 ) ) ;
#2469 = CARTESIAN_POINT ( 'NONE',  ( -5.250000000000000000, -27.37500000000000000, -6.429395695523604153E-16 ) ) ;
#2470 = VERTEX_POINT ( 'NONE', #1422 ) ;
#2471 = CARTESIAN_POINT ( 'NONE',  ( -2.692658234374996518, -28.28645833299193413, 4.663820869356208654 ) ) ;
#2472 = CARTESIAN_POINT ( 'NONE',  ( 3.507514324621434199, -2.050659073900638951, 1.431606283892693066 ) ) ;
#2473 = ORIENTED_EDGE ( 'NONE', *, *, #4027, .F. ) ;
#2474 = CARTESIAN_POINT ( 'NONE',  ( 5.250000000000000000, -27.50000000000000000, 0.000000000000000000 ) ) ;
#2475 = EDGE_CURVE ( 'NONE', #27, #610, #9074, .T. ) ;
#2476 = CARTESIAN_POINT ( 'NONE',  ( -3.507514324621433754, -2.850659073900639218, -1.431606283892695064 ) ) ;
#2477 = ORIENTED_EDGE ( 'NONE', *, *, #4082, .F. ) ;
#2478 = FILL_AREA_STYLE ('',( #3045 ) ) ;
#2479 = FACE_BOUND ( 'NONE', #8500, .T. ) ;
#2480 = ORIENTED_EDGE ( 'NONE', *, *, #1050, .F. ) ;
#2481 = CARTESIAN_POINT ( 'NONE',  ( -5.114683531250000748, -29.00520833367473017, -2.952963913586935440 ) ) ;
#2482 = CARTESIAN_POINT ( 'NONE',  ( 3.007514324621463508, -2.749340926099361759, -1.224499502706076770 ) ) ;
#2483 = CARTESIAN_POINT ( 'NONE',  ( 5.249999999999997335, -28.55208333401612819, 3.031088913245538308 ) ) ;
#2484 = FACE_OUTER_BOUND ( 'NONE', #8918, .T. ) ;
#2485 = CARTESIAN_POINT ( 'NONE',  ( 5.114683531250000748, -28.17187500034139447, 0.000000000000000000 ) ) ;
#2486 = CARTESIAN_POINT ( 'NONE',  ( 1.406733260263391960, -27.33258545099816672, 5.250000000000000000 ) ) ;
#2487 = EDGE_CURVE ( 'NONE', #6849, #8580, #7097, .T. ) ;
#2488 = CARTESIAN_POINT ( 'NONE',  ( 5.249999999999997335, -29.27083333333333570, 3.031088913245538308 ) ) ;
#2489 = CARTESIAN_POINT ( 'NONE',  ( 5.114683531250000748, -27.60937500034139802, 0.000000000000000000 ) ) ;
#2490 = SHAPE_REPRESENTATION ( 'lead sleeve', ( #888 ), #5908 ) ;
#2491 = ORIENTED_EDGE ( 'NONE', *, *, #2832, .F. ) ;
#2492 = DIRECTION ( 'NONE',  ( 0.000000000000000000, -1.000000000000000000, 0.000000000000000000 ) ) ;
#2493 = CARTESIAN_POINT ( 'NONE',  ( 2.692658234375002735, -29.27604166632526983, 4.663820869356205101 ) ) ;
#2494 = FILL_AREA_STYLE ('',( #4585 ) ) ;
#2495 = CARTESIAN_POINT ( 'NONE',  ( 2.692658234374998738, -28.94270833299193413, -4.663820869356206877 ) ) ;
#2496 = ORIENTED_EDGE ( 'NONE', *, *, #9064, .T. ) ;
#2497 = FACE_OUTER_BOUND ( 'NONE', #808, .T. ) ;
#2498 = CARTESIAN_POINT ( 'NONE',  ( -5.250000000000000000, -28.17708333401613174, -3.031088913245536531 ) ) ;
#2499 = STYLED_ITEM ( 'NONE', ( #8555 ), #6298 ) ;
#2500 = CARTESIAN_POINT ( 'NONE',  ( -5.385316468750000141, -29.35937499965859843, 0.000000000000000000 ) ) ;
#2501 = EDGE_LOOP ( 'NONE', ( #7351, #2982, #1065, #4344 ) ) ;
#2502 = CARTESIAN_POINT ( 'NONE',  ( -2.692658234374996518, -28.28645833299193413, 4.663820869356208654 ) ) ;
#2503 = CARTESIAN_POINT ( 'NONE',  ( 1.431606283892694842, -0.8506590739006389956, -3.507514324621434199 ) ) ;
#2504 = CARTESIAN_POINT ( 'NONE',  ( 0.000000000000000000, -30.00000000000000000, 5.250000000000000000 ) ) ;
#2505 = FILL_AREA_STYLE ('',( #2559 ) ) ;
#2506 = DIRECTION ( 'NONE',  ( 0.000000000000000000, 0.000000000000000000, -1.000000000000000000 ) ) ;
#2507 = CARTESIAN_POINT ( 'NONE',  ( 3.500000000000000000, -5.849340926099361404, 0.01814118441321387054 ) ) ;
#2508 = AXIS2_PLACEMENT_3D ( 'NONE', #5155, #2327, #2375 ) ;
#2509 = CARTESIAN_POINT ( 'NONE',  ( -5.114683531250000748, -29.71354166700806232, 2.952963913586931888 ) ) ;
#2510 = CARTESIAN_POINT ( 'NONE',  ( 0.000000000000000000, -50.00000000000000000, -2.786798956483056422 ) ) ;
#2511 = SHAPE_DEFINITION_REPRESENTATION ( #357, #4551 ) ;
#2512 = CARTESIAN_POINT ( 'NONE',  ( 5.385316468750001029, -28.97395833299193413, 3.109213912904135846 ) ) ;
#2513 = EDGE_CURVE ( 'NONE', #8050, #1074, #6394, .T. ) ;
#2514 = CARTESIAN_POINT ( 'NONE',  ( -2.841254879263533262, -2.049340926099361138, 2.815599370228847764 ) ) ;
#2515 = CARTESIAN_POINT ( 'NONE',  ( 0.000000000000000000, -30.00000000000000000, 0.000000000000000000 ) ) ;
#2516 = CARTESIAN_POINT ( 'NONE',  ( -5.385316468750000141, -28.57812499965860198, 0.000000000000000000 ) ) ;
#2517 = CARTESIAN_POINT ( 'NONE',  ( 0.01814118441313990887, -3.350659073900639218, 3.500000000000000000 ) ) ;
#2518 = ORIENTED_EDGE ( 'NONE', *, *, #6208, .F. ) ;
#2519 = CARTESIAN_POINT ( 'NONE',  ( 2.625000000000000444, -27.95833333333333215, -4.546633369868303021 ) ) ;
#2520 = AXIS2_PLACEMENT_3D ( 'NONE', #2121, #4947, #7803 ) ;
#2521 = PRODUCT_RELATED_PRODUCT_CATEGORY ( 'part', '', ( #7829 ) ) ;
#2522 = CARTESIAN_POINT ( 'NONE',  ( -2.487701488670202910, -7.550659073900639839, -2.462045979635629767 ) ) ;
#2523 = CARTESIAN_POINT ( 'NONE',  ( -5.114683531250001636, -27.02604166700806587, 2.952963913586931444 ) ) ;
#2524 = VERTEX_POINT ( 'NONE', #5697 ) ;
#2525=STYLED_ITEM('',(#9225),#8451);
#2526 = CARTESIAN_POINT ( 'NONE',  ( 1.113604000661152470E-15, -28.93749999999999645, 6.062177826491070398 ) ) ;
#2527 = VERTEX_POINT ( 'NONE', #2169 ) ;
#2528 = CARTESIAN_POINT ( 'NONE',  ( 5.114683531250000748, -29.08854166700806942, -2.952963913586932776 ) ) ;
#2529 = CARTESIAN_POINT ( 'NONE',  ( 2.108492589042307408, -0.8493409260993616261, 2.134148098076978251 ) ) ;
#2530 = AXIS2_PLACEMENT_3D ( 'NONE', #6216, #1854, #4589 ) ;
#2531 = CARTESIAN_POINT ( 'NONE',  ( 0.000000000000000000, -53.00000000000000000, 0.000000000000000000 ) ) ;
#2532 = DIRECTION ( 'NONE',  ( -1.000000000000000000, 0.000000000000000000, -0.000000000000000000 ) ) ;
#2533 = CARTESIAN_POINT ( 'NONE',  ( 5.114683531249998971, -29.19270833367473017, 2.952963913586936329 ) ) ;
#2534 = CARTESIAN_POINT ( 'NONE',  ( -5.249999999999997335, -29.97916666666666430, 3.031088913245538308 ) ) ;
#2535 = VECTOR ( 'NONE', #1362, 1000.000000000000000 ) ;
#2536 = CARTESIAN_POINT ( 'NONE',  ( 2.033577675846918216E-14, -27.84375000068279959, 5.250000000000000888 ) ) ;
#2537 = DIRECTION ( 'NONE',  ( 0.000000000000000000, 1.000000000000000000, 0.000000000000000000 ) ) ;
#2538 = ADVANCED_BREP_SHAPE_REPRESENTATION ( '', ( #5399, #888 ), #7241 ) ;
#2539 = CIRCLE ( 'NONE', #7592, 2.500000000000000000 ) ;
#2540 = ORIENTED_EDGE ( 'NONE', *, *, #4138, .F. ) ;
#2541 = DIRECTION ( 'NONE',  ( 0.000000000000000000, 0.000000000000000000, 1.000000000000000000 ) ) ;
#2542 = CARTESIAN_POINT ( 'NONE',  ( -2.692658234375000514, -28.40104166632526628, -4.663820869356205989 ) ) ;
#2543 = CARTESIAN_POINT ( 'NONE',  ( -5.250000000000000000, -28.62499999999999645, -6.429395695523604153E-16 ) ) ;
#2544 = DIRECTION ( 'NONE',  ( 0.000000000000000000, 0.000000000000000000, 1.000000000000000000 ) ) ;
#2545 = CARTESIAN_POINT ( 'NONE',  ( 2.692658234375002735, -29.27604166632526983, 4.663820869356205101 ) ) ;
#2546 = CARTESIAN_POINT ( 'NONE',  ( 2.487701488670255756, -1.249340926099361093, -2.462045979635577364 ) ) ;
#2547 = VERTEX_POINT ( 'NONE', #7847 ) ;
#2548 = AXIS2_PLACEMENT_3D ( 'NONE', #432, #2537, #8937 ) ;
#2549 = EDGE_CURVE ( 'NONE', #5349, #2876, #1465, .T. ) ;
#2550 = PLANE ( 'NONE',  #8924 ) ;
#2551 = CARTESIAN_POINT ( 'NONE',  ( -2.624999999999998668, -28.19791666734946389, -4.546633369868303021 ) ) ;
#2552 = AXIS2_PLACEMENT_3D ( 'NONE', #6080, #1815, #3168 ) ;
#2553 = CARTESIAN_POINT ( 'NONE',  ( -2.692658234375000514, -29.15104166632526983, -4.663820869356205989 ) ) ;
#2554 = ORIENTED_EDGE ( 'NONE', *, *, #3417, .F. ) ;
#2555 = CIRCLE ( 'NONE', #5803, 6.250000000000000000 ) ;
#2556 = CARTESIAN_POINT ( 'NONE',  ( -5.385316468749998364, -28.55729166632527338, 3.109213912904140287 ) ) ;
#2557 = CARTESIAN_POINT ( 'NONE',  ( 3.000000000000000444, -6.950659073900640195, -0.01814118441314496039 ) ) ;
#2558 = CYLINDRICAL_SURFACE ( 'NONE', #129, 5.250000000000000000 ) ;
#2559 = FILL_AREA_STYLE_COLOUR ( '', #6693 ) ;
#2560 = DIRECTION ( 'NONE',  ( 0.000000000000000000, 1.000000000000000000, 0.000000000000000000 ) ) ;
#2561 = ADVANCED_FACE ( 'NONE', ( #303, #5931 ), #2261, .F. ) ;
#2562 = CARTESIAN_POINT ( 'NONE',  ( 1.406733260263391960, -28.08258545099816672, 5.250000000000000000 ) ) ;
#2563 = B_SPLINE_CURVE_WITH_KNOTS ( 'NONE', 3,
 ( #6467, #894, #4530, #1498 ),
 .UNSPECIFIED., .F., .F.,
 ( 4, 4 ),
 ( 0.008580651465885628590, 0.01459740681124464291 ),
 .UNSPECIFIED. ) ;
#2564 = CARTESIAN_POINT ( 'NONE',  ( 5.114683531249998971, -29.38020833367473017, 2.952963913586936329 ) ) ;
#2565 = VERTEX_POINT ( 'NONE', #5184 ) ;
#2566 = APPLICATION_PROTOCOL_DEFINITION ( 'draft international standard', 'automotive_design', 1998, #4038 ) ;
#2567 = CARTESIAN_POINT ( 'NONE',  ( -5.385316468750000141, -29.82812499965859843, 0.000000000000000000 ) ) ;
#2568 = EDGE_CURVE ( 'NONE', #6698, #2524, #6575, .T. ) ;
#2569 = CARTESIAN_POINT ( 'NONE',  ( -2.462045979635576920, -8.049340926099361582, -2.487701488670255756 ) ) ;
#2570 = CARTESIAN_POINT ( 'NONE',  ( -5.249999999999999112, -29.52083333333333215, -3.031088913245534755 ) ) ;
#2571 = CARTESIAN_POINT ( 'NONE',  ( 1.142306659890740623E-15, -28.76562499965860553, 6.218427825808274356 ) ) ;
#2572 = EDGE_CURVE ( 'NONE', #8745, #2851, #7536, .T. ) ;
#2573 = CARTESIAN_POINT ( 'NONE',  ( -2.487701488670202910, -7.550659073900639839, -2.462045979635629767 ) ) ;
#2574 = ORIENTED_EDGE ( 'NONE', *, *, #3984, .F. ) ;
#2575 = DIRECTION ( 'NONE',  ( 0.000000000000000000, 0.000000000000000000, -1.000000000000000000 ) ) ;
#2576 = CARTESIAN_POINT ( 'NONE',  ( -1.431606283892693066, -1.650659073900639040, 3.507514324621434199 ) ) ;
#2577 = ORIENTED_EDGE ( 'NONE', *, *, #4348, .T. ) ;
#2578 = CARTESIAN_POINT ( 'NONE',  ( 1.113604000661152470E-15, -28.18750000000000000, 6.062177826491070398 ) ) ;
#2579 = CONICAL_SURFACE ( 'NONE', #6132, 2.000000000000000000, 0.06981317007977333455 ) ;
#2580 = ORIENTED_EDGE ( 'NONE', *, *, #4211, .F. ) ;
#2581 = CARTESIAN_POINT ( 'NONE',  ( 5.114683531249998971, -29.13020833367473017, 2.952963913586936329 ) ) ;
#2582 = CARTESIAN_POINT ( 'NONE',  ( -3.492485675378536047, -8.149340926099361226, -1.467888652719048670 ) ) ;
#2583 = DIRECTION ( 'NONE',  ( 0.000000000000000000, -1.000000000000000000, 0.000000000000000000 ) ) ;
#2584 = CARTESIAN_POINT ( 'NONE',  ( 5.114683531250000748, -27.42187500034139802, 0.000000000000000000 ) ) ;
#2585 = FACE_BOUND ( 'NONE', #4396, .T. ) ;
#2586 = AXIS2_PLACEMENT_3D ( 'NONE', #5804, #5243, #5941 ) ;
#2587 = MECHANICAL_DESIGN_GEOMETRIC_PRESENTATION_REPRESENTATION (  '', ( #8813 ), #47 ) ;
#2588 = CARTESIAN_POINT ( 'NONE',  ( 1.185285273922203525E-14, -29.18750000000000000, -5.250000000000000000 ) ) ;
#2589 = CARTESIAN_POINT ( 'NONE',  ( -1.084901341431563923E-15, -27.42187500034139802, 5.905927827173866440 ) ) ;
#2590 = CARTESIAN_POINT ( 'NONE',  ( -5.114683531249999859, -29.31770833367473372, -2.952963913586935440 ) ) ;
#2591 = CIRCLE ( 'NONE', #5546, 1.750000000000000222 ) ;
#2592 = CARTESIAN_POINT ( 'NONE',  ( 1.406733260263395735, -27.92633545031536713, 5.250000000000000000 ) ) ;
#2593 = ADVANCED_FACE ( 'NONE', ( #3065 ), #8027, .T. ) ;
#2594 = CARTESIAN_POINT ( 'NONE',  ( 2.692658234374998738, -28.19270833299193413, -4.663820869356206877 ) ) ;
#2595 = CARTESIAN_POINT ( 'NONE',  ( -2.692658234375000514, -29.90104166632526983, -4.663820869356205989 ) ) ;
#2596 = VECTOR ( 'NONE', #3638, 1000.000000000000000 ) ;
#2597 = SURFACE_SIDE_STYLE ('',( #8992 ) ) ;
#2598 = CARTESIAN_POINT ( 'NONE',  ( 2.692658234375002735, -29.02604166632526983, 4.663820869356205101 ) ) ;
#2599 = CARTESIAN_POINT ( 'NONE',  ( -1.431606283892620235, -3.149340926099361671, -3.507514324621463953 ) ) ;
#2600 = VERTEX_POINT ( 'NONE', #8678 ) ;
#2601 = CARTESIAN_POINT ( 'NONE',  ( -5.249999999999997335, -27.47916666666666430, 3.031088913245538308 ) ) ;
#2602 = CARTESIAN_POINT ( 'NONE',  ( 5.250000000000000000, -27.53125000068279604, 0.000000000000000000 ) ) ;
#2603 = CARTESIAN_POINT ( 'NONE',  ( 2.692658234375002735, -29.77604166632526983, 4.663820869356205101 ) ) ;
#2604 = CONICAL_SURFACE ( 'NONE', #207, 3.500000000000000444, 0.08726646259971666819 ) ;
#2605 = EDGE_CURVE ( 'NONE', #3879, #8235, #2967, .T. ) ;
#2606 = ORIENTED_EDGE ( 'NONE', *, *, #5013, .T. ) ;
#2607 = CARTESIAN_POINT ( 'NONE',  ( -5.385316468749998364, -27.80729166632526628, 3.109213912904140287 ) ) ;
#2608 = CARTESIAN_POINT ( 'NONE',  ( -3.507514324621434199, -2.850659073900639662, -1.431606283892695064 ) ) ;
#2609 = FACE_OUTER_BOUND ( 'NONE', #1627, .T. ) ;
#2610 =( BOUNDED_CURVE ( )  B_SPLINE_CURVE ( 2, ( #5276, #953, #1702, #8073, #5928, #2308, #4495, #7190, #6625 ),
 .UNSPECIFIED., .F., .F. ) 
 B_SPLINE_CURVE_WITH_KNOTS ( ( 3, 2, 2, 2, 3 ),
 ( 0.2708333333333333148, 0.2777777777777777901, 0.2916666666666666852, 0.3055555555555555802, 0.3125000000000000000 ),
 .UNSPECIFIED. ) 
 CURVE ( )  GEOMETRIC_REPRESENTATION_ITEM ( )  RATIONAL_B_SPLINE_CURVE ( ( 0.9330127018922194093, 0.9330127018922190762, 1.000000000000000000, 0.8660254037844387076, 1.000000000000000000, 0.8660254037844387076, 1.000000000000000000, 0.9330127018922194093, 0.9330127018922194093 ) ) 
 REPRESENTATION_ITEM ( '' )  );
#2611 = CARTESIAN_POINT ( 'NONE',  ( -5.249999999999999112, -28.45833333265053611, -3.031088913245534755 ) ) ;
#2612 = CARTESIAN_POINT ( 'NONE',  ( 0.000000000000000000, -20.00000000000000000, 0.000000000000000000 ) ) ;
#2613 =( REPRESENTATION_RELATIONSHIP ('NONE','NONE', #735, #4384 ) REPRESENTATION_RELATIONSHIP_WITH_TRANSFORMATION ( #7628 )SHAPE_REPRESENTATION_RELATIONSHIP( ) );
#2614 = PLANE ( 'NONE',  #4076 ) ;
#2615 = EDGE_LOOP ( 'NONE', ( #3150, #8031, #999, #2255, #1305, #7191 ) ) ;
#2616 = SHAPE_DEFINITION_REPRESENTATION ( #4672, #3200 ) ;
#2617 = CARTESIAN_POINT ( 'NONE',  ( -5.385316468749998364, -29.05729166632526628, 3.109213912904140287 ) ) ;
#2618 = CARTESIAN_POINT ( 'NONE',  ( 0.01814118441321408565, -3.049340926099361138, -3.500000000000000000 ) ) ;
#2619 = CARTESIAN_POINT ( 'NONE',  ( -5.250000000000000000, -28.00000000000000000, 0.000000000000000000 ) ) ;
#2620 = CARTESIAN_POINT ( 'NONE',  ( -2.692658234374996518, -29.78645833299193413, 4.663820869356208654 ) ) ;
#2621 = CARTESIAN_POINT ( 'NONE',  ( -2.487701488670202910, -2.750659073900639129, -2.462045979635629767 ) ) ;
#2622 = ORIENTED_EDGE ( 'NONE', *, *, #1762, .F. ) ;
#2623 = CARTESIAN_POINT ( 'NONE',  ( -5.250000000000000000, -27.14583333333333570, -3.031088913245536531 ) ) ;
#2624 = CARTESIAN_POINT ( 'NONE',  ( 0.000000000000000000, -27.00000000000000000, 0.000000000000000000 ) ) ;
#2625 = CARTESIAN_POINT ( 'NONE',  ( 3.507514324621434199, -0.4506590739006389734, 1.431606283892693066 ) ) ;
#2626 = EDGE_CURVE ( 'NONE', #610, #8948, #7980, .T. ) ;
#2627 = VERTEX_POINT ( 'NONE', #2402 ) ;
#2628 = CARTESIAN_POINT ( 'NONE',  ( 5.250000000000000000, -28.60416666666666430, -3.031088913245536531 ) ) ;
#2629 = ORIENTED_EDGE ( 'NONE', *, *, #6612, .T. ) ;
#2630 = CARTESIAN_POINT ( 'NONE',  ( -1.084901341431563726E-15, -28.92187500034139447, 5.905927827173866440 ) ) ;
#2631 = CARTESIAN_POINT ( 'NONE',  ( 3.507514324621465285, -7.549340926099362470, -1.431606283892619125 ) ) ;
#2632 = LINE ( 'NONE', #1738, #6720 ) ;
#2633 = CARTESIAN_POINT ( 'NONE',  ( 5.114683531249999859, -27.15104166700806232, -2.952963913586932776 ) ) ;
#2634 = CARTESIAN_POINT ( 'NONE',  ( 3.616337804771879580E-16, -27.54687500034140157, -5.905927827173866440 ) ) ;
#2635 = DIRECTION ( 'NONE',  ( 0.000000000000000000, 0.000000000000000000, 1.000000000000000000 ) ) ;
#2636 = CARTESIAN_POINT ( 'NONE',  ( 3.616337804771879580E-16, -28.85937500034139802, -5.905927827173866440 ) ) ;
#2637 = LINE ( 'NONE', #8211, #3853 ) ;
#2638 = EDGE_CURVE ( 'NONE', #3248, #4378, #4326, .T. ) ;
#2639 = CARTESIAN_POINT ( 'NONE',  ( 5.385316468750000141, -28.98437499965859843, -6.595110575850215044E-16 ) ) ;
#2640 = CARTESIAN_POINT ( 'NONE',  ( 6.972266317189433020E-16, -29.21875000068279249, -5.250000000000000000 ) ) ;
#2641 = CARTESIAN_POINT ( 'NONE',  ( 5.385316468749999252, -29.21354166632526628, -3.109213912904139399 ) ) ;
#2642 = CARTESIAN_POINT ( 'NONE',  ( -3.492485675378536047, -4.949340926099361049, -1.467888652719048670 ) ) ;
#2643 = CARTESIAN_POINT ( 'NONE',  ( -3.500000000000000000, -1.849340926099361182, -0.01814118441321344033 ) ) ;
#2644 = ORIENTED_EDGE ( 'NONE', *, *, #8333, .T. ) ;
#2645 = CARTESIAN_POINT ( 'NONE',  ( 0.000000000000000000, -29.00000000000000355, -2.629341307491595447 ) ) ;
#2646 = CARTESIAN_POINT ( 'NONE',  ( 2.624999999999996891, -28.57291666734946389, 4.546633369868304797 ) ) ;
#2647 = CARTESIAN_POINT ( 'NONE',  ( -5.385316468750001029, -29.88020833299193413, -3.109213912904136734 ) ) ;
#2648 = ORIENTED_EDGE ( 'NONE', *, *, #2843, .F. ) ;
#2649 = CARTESIAN_POINT ( 'NONE',  ( 1.142306659890740623E-15, -27.76562499965860198, 6.218427825808274356 ) ) ;
#2650 = CARTESIAN_POINT ( 'NONE',  ( 3.500000000000000000, -3.750659073900639129, -0.01814118441313969030 ) ) ;
#2651 = DIRECTION ( 'NONE',  ( 0.000000000000000000, 0.000000000000000000, -1.000000000000000000 ) ) ;
#2652 =( NAMED_UNIT ( * ) PLANE_ANGLE_UNIT ( ) SI_UNIT ( $, .RADIAN. ) );
#2653 = CARTESIAN_POINT ( 'NONE',  ( 1.406733260263391960, -28.30133545031536713, 5.250000000000000000 ) ) ;
#2654 = CARTESIAN_POINT ( 'NONE',  ( 5.249999999999999112, -28.01041666734946389, -3.031088913245534755 ) ) ;
#2655 = DIRECTION ( 'NONE',  ( 0.000000000000000000, -1.000000000000000000, 0.000000000000000000 ) ) ;
#2656 = DIRECTION ( 'NONE',  ( 0.000000000000000000, 0.000000000000000000, -1.000000000000000000 ) ) ;
#2657 = CONTEXT_DEPENDENT_SHAPE_REPRESENTATION ( #3854, #7648 ) ;
#2658 = AXIS2_PLACEMENT_3D ( 'NONE', #875, #3725, #3169 ) ;
#2659 = CARTESIAN_POINT ( 'NONE',  ( 5.385316468749999252, -29.43229166632526983, -3.109213912904139399 ) ) ;
#2660 = CARTESIAN_POINT ( 'NONE',  ( -3.500000000000000000, -3.449340926099361049, -0.01814118441321344033 ) ) ;
#2661 =( BOUNDED_CURVE ( )  B_SPLINE_CURVE ( 2, ( #6777, #9052, #403, #6178, #550, #1250, #5328, #6829, #4045 ),
 .UNSPECIFIED., .F., .F. ) 
 B_SPLINE_CURVE_WITH_KNOTS ( ( 3, 2, 2, 2, 3 ),
 ( 0.1458333333333333426, 0.1527777777777777901, 0.1666666666666666574, 0.1805555555555555525, 0.1875000000000000000 ),
 .UNSPECIFIED. ) 
 CURVE ( )  GEOMETRIC_REPRESENTATION_ITEM ( )  RATIONAL_B_SPLINE_CURVE ( ( 0.9330127018922194093, 0.9330127018922194093, 1.000000000000000000, 0.8660254037844387076, 1.000000000000000000, 0.8660254037844387076, 1.000000000000000000, 0.9330127018922194093, 0.9330127018922194093 ) ) 
 REPRESENTATION_ITEM ( '' )  );
#2662 = FACE_OUTER_BOUND ( 'NONE', #5906, .T. ) ;
#2663 = CARTESIAN_POINT ( 'NONE',  ( 5.385316468750001029, -29.72395833299193413, 3.109213912904135846 ) ) ;
#2664 = CARTESIAN_POINT ( 'NONE',  ( 2.487701488670203354, -1.950659073900639084, 2.462045979635629323 ) ) ;
#2665 = CARTESIAN_POINT ( 'NONE',  ( 8.603239422292019767E-08, -29.99999999999999645, -5.249999999999998224 ) ) ;
#2666 = CYLINDRICAL_SURFACE ( 'NONE', #1649, 4.250000000000000000 ) ;
#2667 = ADVANCED_FACE ( 'NONE', ( #1705, #6583 ), #7375, .T. ) ;
#2668 = CARTESIAN_POINT ( 'NONE',  ( -3.507514324621433754, -4.450659073900639306, -1.431606283892695064 ) ) ;
#2669 = ORIENTED_EDGE ( 'NONE', *, *, #7652, .F. ) ;
#2670 = FILL_AREA_STYLE ('',( #4706 ) ) ;
#2671 = CARTESIAN_POINT ( 'NONE',  ( 5.250000000000000000, -27.85416666666666430, -3.031088913245536531 ) ) ;
#2672 = CARTESIAN_POINT ( 'NONE',  ( 3.616337804771879580E-16, -27.04687500034139802, -5.905927827173866440 ) ) ;
#2673 = CARTESIAN_POINT ( 'NONE',  ( 1.224499502706077214, -0.7493409260993615373, 3.007514324621463508 ) ) ;
#2674 = CARTESIAN_POINT ( 'NONE',  ( -2.557341765625002594, -27.25520833367473017, 4.429445870380399164 ) ) ;
#2675 = DIRECTION ( 'NONE',  ( 0.000000000000000000, 1.000000000000000000, 0.000000000000000000 ) ) ;
#2676 = CARTESIAN_POINT ( 'NONE',  ( -5.114683531250000748, -29.04687500034139802, -6.263680815196995234E-16 ) ) ;
#2677 = AXIS2_PLACEMENT_3D ( 'NONE', #8411, #634, #5035 ) ;
#2678 = CARTESIAN_POINT ( 'NONE',  ( -2.557341765624999042, -29.08854166700806587, -4.429445870380400052 ) ) ;
#2679 = CARTESIAN_POINT ( 'NONE',  ( 0.000000000000000000, -20.00000000000000000, 0.000000000000000000 ) ) ;
#2680 = CARTESIAN_POINT ( 'NONE',  ( -3.712013335537174572E-16, -29.24999999931720396, -6.062177826491070398 ) ) ;
#2681 = FACE_OUTER_BOUND ( 'NONE', #1029, .T. ) ;
#2682 = CYLINDRICAL_SURFACE ( 'NONE', #4305, 6.250000000000000000 ) ;
#2683 = CARTESIAN_POINT ( 'NONE',  ( -2.692658234374996518, -29.56770833299193413, 4.663820869356208654 ) ) ;
#2684 = CARTESIAN_POINT ( 'NONE',  ( -3.500000000000000000, -1.849340926099361182, -0.01814118441321344033 ) ) ;
#2685 = AXIS2_PLACEMENT_3D ( 'NONE', #8707, #101, #1641 ) ;
#2686 = CLOSED_SHELL ( 'NONE', ( #8780, #4900, #2740, #3301, #7354, #1360, #6740, #5728, #3114, #3810, #5162, #9032, #5050 ) ) ;
#2687 = CARTESIAN_POINT ( 'NONE',  ( 0.01814118441321408565, -1.449340926099361271, -3.500000000000000000 ) ) ;
#2688 = ORIENTED_EDGE ( 'NONE', *, *, #5430, .F. ) ;
#2689 = DIRECTION ( 'NONE',  ( 0.000000000000000000, 0.000000000000000000, 1.000000000000000000 ) ) ;
#2690 = VECTOR ( 'NONE', #7111, 1000.000000000000000 ) ;
#2691 = CARTESIAN_POINT ( 'NONE',  ( -2.625000000000002220, -27.61458333401612819, 4.546633369868302132 ) ) ;
#2692 = CARTESIAN_POINT ( 'NONE',  ( -2.692658234375000514, -29.40104166632526983, -4.663820869356205989 ) ) ;
#2693 = VERTEX_POINT ( 'NONE', #4445 ) ;
#2694 = CARTESIAN_POINT ( 'NONE',  ( -1.975475456537005874E-15, -29.56250000000000000, 5.249999999999999112 ) ) ;
#2695 = CARTESIAN_POINT ( 'NONE',  ( 3.007514324621436863, -6.850659073900641438, 1.224499502706140719 ) ) ;
#2696 = CYLINDRICAL_SURFACE ( 'NONE', #8459, 5.250000000000000000 ) ;
#2697 = VECTOR ( 'NONE', #4369, 1000.000000000000000 ) ;
#2698 = DIRECTION ( 'NONE',  ( 0.000000000000000000, 0.000000000000000000, 1.000000000000000000 ) ) ;
#2699 = CARTESIAN_POINT ( 'NONE',  ( 0.000000000000000000, 69.99999999999998579, 5.250000000000000000 ) ) ;
#2700 = CARTESIAN_POINT ( 'NONE',  ( -0.01814118441321365544, -7.049340926099361582, 3.500000000000000000 ) ) ;
#2701 = CARTESIAN_POINT ( 'NONE',  ( -5.114683531250000748, -28.21354166700806232, 2.952963913586931888 ) ) ;
#2702 = LINE ( 'NONE', #1383, #6416 ) ;
#2703 = CARTESIAN_POINT ( 'NONE',  ( -5.385316468749998364, -29.30729166632526983, 3.109213912904140287 ) ) ;
#2704 = CARTESIAN_POINT ( 'NONE',  ( -3.500000000000000000, -5.049340926099361582, -0.01814118441321344033 ) ) ;
#2705 = CARTESIAN_POINT ( 'NONE',  ( 0.000000000000000000, -46.00000000000000000, 0.000000000000000000 ) ) ;
#2706 = CARTESIAN_POINT ( 'NONE',  ( 1.142306659890740623E-15, -29.76562499965859843, 6.218427825808274356 ) ) ;
#2707 = EDGE_CURVE ( 'NONE', #6263, #4547, #3442, .T. ) ;
#2708 = CARTESIAN_POINT ( 'NONE',  ( 2.815599370228907716, -5.550659073900638063, -2.841254879263473310 ) ) ;
#2709 = CARTESIAN_POINT ( 'NONE',  ( 5.249999999999999112, -27.02083333333333570, 3.031088913245538308 ) ) ;
#2710 = CARTESIAN_POINT ( 'NONE',  ( -2.324088772396477476E-15, -29.68750000000000000, -5.250000000000000000 ) ) ;
#2711 = EDGE_CURVE ( 'NONE', #3105, #8178, #3980, .T. ) ;
#2712 = ADVANCED_FACE ( 'NONE', ( #5321 ), #6171, .T. ) ;
#2713 = VERTEX_POINT ( 'NONE', #2645 ) ;
#2714 =( LENGTH_UNIT ( ) NAMED_UNIT ( * ) SI_UNIT ( .MILLI., .METRE. ) );
#2715 = CARTESIAN_POINT ( 'NONE',  ( -3.712013335537174572E-16, -28.31250000000000355, -6.062177826491070398 ) ) ;
#2716 = VERTEX_POINT ( 'NONE', #5517 ) ;
#2717 = CARTESIAN_POINT ( 'NONE',  ( 2.557341765625000818, -27.56770833367473017, -4.429445870380400052 ) ) ;
#2718 = CARTESIAN_POINT ( 'NONE',  ( 2.992485675378538712, -5.749340926099361759, 1.260781871532494103 ) ) ;
#2719 = CARTESIAN_POINT ( 'NONE',  ( -2.557341765625002594, -28.00520833367473017, 4.429445870380399164 ) ) ;
#2720 = CARTESIAN_POINT ( 'NONE',  ( 0.000000000000000000, -9.000000000000000000, 0.000000000000000000 ) ) ;
#2721 = CARTESIAN_POINT ( 'NONE',  ( 2.557341765625000818, -28.63020833367473017, -4.429445870380400052 ) ) ;
#2722 = CARTESIAN_POINT ( 'NONE',  ( -2.557341765624999042, -29.33854166700806232, -4.429445870380400052 ) ) ;
#2723 = DIRECTION ( 'NONE',  ( 0.000000000000000000, 1.000000000000000000, 0.000000000000000000 ) ) ;
#2724 = CARTESIAN_POINT ( 'NONE',  ( 2.625000000000002220, -28.85416666598386826, 4.546633369868302132 ) ) ;
#2725 = CARTESIAN_POINT ( 'NONE',  ( 2.692658234375002735, -29.52604166632526983, 4.663820869356205101 ) ) ;
#2726 = CARTESIAN_POINT ( 'NONE',  ( 6.429395695523604153E-16, 69.99999999999998579, -5.250000000000000000 ) ) ;
#2727 = CIRCLE ( 'NONE', #5676, 6.250000000000000000 ) ;
#2728 = CARTESIAN_POINT ( 'NONE',  ( -5.250000000000000000, -27.00000000000000000, 0.000000000000000000 ) ) ;
#2729 = CARTESIAN_POINT ( 'NONE',  ( -3.492485675378536047, -3.349340926099361404, -1.467888652719048670 ) ) ;
#2730 = CARTESIAN_POINT ( 'NONE',  ( 1.674995433905601239, -7.749340926099362648, -3.992485675378532939 ) ) ;
#2731 = CIRCLE ( 'NONE', #2874, 2.500000000000000000 ) ;
#2732 = ORIENTED_EDGE ( 'NONE', *, *, #4401, .T. ) ;
#2733 = APPLICATION_CONTEXT ( 'automotive_design' ) ;
#2734 = DIRECTION ( 'NONE',  ( 0.000000000000000000, 0.000000000000000000, -1.000000000000000000 ) ) ;
#2735 = CARTESIAN_POINT ( 'NONE',  ( -1.113604000661152470E-15, -27.09375000068279604, 6.062177826491070398 ) ) ;
#2736 = EDGE_CURVE ( 'NONE', #2202, #7225, #7481, .T. ) ;
#2737 = CARTESIAN_POINT ( 'NONE',  ( -5.250000000000000000, -27.18749999931720396, 0.000000000000000000 ) ) ;
#2738 = VECTOR ( 'NONE', #6424, 1000.000000000000000 ) ;
#2739 =( BOUNDED_CURVE ( )  B_SPLINE_CURVE ( 2, ( #4311, #4990, #1379, #2038, #2835, #6439, #3439, #2123, #770 ),
 .UNSPECIFIED., .F., .F. ) 
 B_SPLINE_CURVE_WITH_KNOTS ( ( 3, 2, 2, 2, 3 ),
 ( 0.6458333333333333703, 0.6527777777777777901, 0.6666666666666666297, 0.6805555555555555802, 0.6875000000000000000 ),
 .UNSPECIFIED. ) 
 CURVE ( )  GEOMETRIC_REPRESENTATION_ITEM ( )  RATIONAL_B_SPLINE_CURVE ( ( 0.9330127018922192983, 0.9330127018922198534, 1.000000000000000000, 0.8660254037844387076, 1.000000000000000000, 0.8660254037844387076, 1.000000000000000000, 0.9330127018922194093, 0.9330127018922194093 ) ) 
 REPRESENTATION_ITEM ( '' )  );
#2740 = ADVANCED_FACE ( 'NONE', ( #8267 ), #2550, .T. ) ;
#2741 = AXIS2_PLACEMENT_3D ( 'NONE', #6157, #3930, #4669 ) ;
#2742 = ORIENTED_EDGE ( 'NONE', *, *, #5944, .F. ) ;
#2743 = CARTESIAN_POINT ( 'NONE',  ( 5.385316468749999252, -29.68229166632527338, -3.109213912904138954 ) ) ;
#2744 = CARTESIAN_POINT ( 'NONE',  ( -0.01814118441313947866, -5.750659073900639129, -3.500000000000000000 ) ) ;
#2745 = DIRECTION ( 'NONE',  ( 0.000000000000000000, -1.000000000000000000, 0.000000000000000000 ) ) ;
#2746 = LINE ( 'NONE', #7895, #2241 ) ;
#2747 = FACE_OUTER_BOUND ( 'NONE', #6001, .T. ) ;
#2748 = CARTESIAN_POINT ( 'NONE',  ( 1.467888652719048226, -6.149340926099361226, -3.492485675378535603 ) ) ;
#2749 = CARTESIAN_POINT ( 'NONE',  ( -5.114683531250000748, -29.21354166700806587, 2.952963913586931888 ) ) ;
#2750 = CARTESIAN_POINT ( 'NONE',  ( -2.624999999999996891, -28.14583333265053255, 4.546633369868304797 ) ) ;
#2751 = CARTESIAN_POINT ( 'NONE',  ( 0.000000000000000000, -30.00000000000000000, 0.000000000000000000 ) ) ;
#2752 = CARTESIAN_POINT ( 'NONE',  ( 1.224499502706077214, -0.7493409260993615373, 3.007514324621463508 ) ) ;
#2753 = APPLICATION_CONTEXT ( 'automotive_design' ) ;
#2754 = CARTESIAN_POINT ( 'NONE',  ( 4.714834644010547828E-16, -20.00000000000000000, 3.500000000000000444 ) ) ;
#2755 = CARTESIAN_POINT ( 'NONE',  ( -5.385316468750001029, -29.34895833299193413, -3.109213912904136734 ) ) ;
#2756 = CARTESIAN_POINT ( 'NONE',  ( 4.000000000000000000, -0.5506590739006383961, -0.01814118441313441674 ) ) ;
#2757 = CARTESIAN_POINT ( 'NONE',  ( 5.250000000000000000, -30.06249999931720041, -6.429395695523604153E-16 ) ) ;
#2758 = PRODUCT_DEFINITION_SHAPE ( 'NONE', 'NONE',  #9196 ) ;
#2759 = DIRECTION ( 'NONE',  ( 0.000000000000000000, -1.000000000000000000, 0.000000000000000000 ) ) ;
#2760 = DIRECTION ( 'NONE',  ( 0.000000000000000000, -1.000000000000000000, 0.000000000000000000 ) ) ;
#2761 = ORIENTED_EDGE ( 'NONE', *, *, #8274, .T. ) ;
#2762 = SURFACE_SIDE_STYLE ('',( #1881 ) ) ;
#2763 = CARTESIAN_POINT ( 'NONE',  ( 2.624999999999998668, -29.83333333333333215, -4.546633369868303021 ) ) ;
#2764 = CARTESIAN_POINT ( 'NONE',  ( -2.557341765624999042, -27.02604166700806232, -4.429445870380400052 ) ) ;
#2765 = CARTESIAN_POINT ( 'NONE',  ( -0.01814118441320841310, -5.449340926099361937, 3.000000000000000444 ) ) ;
#2766 = CARTESIAN_POINT ( 'NONE',  ( -5.114683531250000748, -27.54687500034139802, -6.263680815196995234E-16 ) ) ;
#2767 = CARTESIAN_POINT ( 'NONE',  ( 0.000000000000000000, -30.00000000000000000, 0.000000000000000000 ) ) ;
#2768 = ADVANCED_FACE ( 'NONE', ( #2497 ), #4083, .T. ) ;
#2769 = CARTESIAN_POINT ( 'NONE',  ( -2.557341765624999042, -28.58854166700806587, -4.429445870380400052 ) ) ;
#2770 = CARTESIAN_POINT ( 'NONE',  ( 6.429395695523604153E-16, -30.00000000000000000, -5.250000000000000000 ) ) ;
#2771 = CARTESIAN_POINT ( 'NONE',  ( 2.557341765624996821, -28.46354166700806587, 4.429445870380401828 ) ) ;
#2772 = CARTESIAN_POINT ( 'NONE',  ( -2.624999999999996891, -28.70833333333333215, 4.546633369868304797 ) ) ;
#2773 = CARTESIAN_POINT ( 'NONE',  ( 1.113604000661152470E-15, -28.62499999931720041, 6.062177826491070398 ) ) ;
#2774 = CARTESIAN_POINT ( 'NONE',  ( 6.429395695523604153E-16, -9.999999999999998224, -5.250000000000000000 ) ) ;
#2775 = CYLINDRICAL_SURFACE ( 'NONE', #9102, 6.250000000000000000 ) ;
#2776 = CARTESIAN_POINT ( 'NONE',  ( -2.462045979635576920, -4.849340926099361404, -2.487701488670255756 ) ) ;
#2777 = CARTESIAN_POINT ( 'NONE',  ( -2.487701488670255312, -6.849340926099361404, 2.462045979635577808 ) ) ;
#2778 = EDGE_CURVE ( 'NONE', #6849, #1943, #8193, .T. ) ;
#2779 = VERTEX_POINT ( 'NONE', #6918 ) ;
#2780 = CARTESIAN_POINT ( 'NONE',  ( -5.317658234375000070, -30.14843749948790119, 0.000000000000000000 ) ) ;
#2781 = CARTESIAN_POINT ( 'NONE',  ( -5.114683531250000748, -29.71354166700806232, 2.952963913586931888 ) ) ;
#2782 = ADVANCED_FACE ( 'NONE', ( #8360 ), #397, .T. ) ;
#2783 = ORIENTED_EDGE ( 'NONE', *, *, #5363, .T. ) ;
#2784 = CARTESIAN_POINT ( 'NONE',  ( 2.692658234375002735, -28.99479166632526983, 4.663820869356205101 ) ) ;
#2785 = CARTESIAN_POINT ( 'NONE',  ( 0.01814118441313467001, -0.1506590739006384849, 4.000000000000000000 ) ) ;
#2786 = DIRECTION ( 'NONE',  ( 0.000000000000000000, -1.000000000000000000, 0.000000000000000000 ) ) ;
#2787 = EDGE_LOOP ( 'NONE', ( #1266, #590 ) ) ;
#2788 = CARTESIAN_POINT ( 'NONE',  ( 0.000000000000000000, 70.00000000000000000, 0.000000000000000000 ) ) ;
#2789 = LINE ( 'NONE', #5040, #7330 ) ;
#2790 = CARTESIAN_POINT ( 'NONE',  ( 0.000000000000000000, -53.00000000000000000, 0.000000000000000000 ) ) ;
#2791 = SHAPE_REPRESENTATION ( 'cap', ( #888 ), #7241 ) ;
#2792 = CARTESIAN_POINT ( 'NONE',  ( -2.557341765625002594, -28.19270833367473017, 4.429445870380399164 ) ) ;
#2793 = FACE_OUTER_BOUND ( 'NONE', #807, .T. ) ;
#2794 = CONTEXT_DEPENDENT_SHAPE_REPRESENTATION ( #6226, #6744 ) ;
#2795 = CARTESIAN_POINT ( 'NONE',  ( -2.624999999999996891, -28.64583333265053611, 4.546633369868304797 ) ) ;
#2796 = CARTESIAN_POINT ( 'NONE',  ( 1.224499502706077214, -5.549340926099361582, 3.007514324621463508 ) ) ;
#2797 = CARTESIAN_POINT ( 'NONE',  ( -1.406733260263395735, -28.10491455036742536, 5.250000000000000000 ) ) ;
#2798 =( GEOMETRIC_REPRESENTATION_CONTEXT ( 3 ) GLOBAL_UNCERTAINTY_ASSIGNED_CONTEXT ( ( #3022 ) ) GLOBAL_UNIT_ASSIGNED_CONTEXT ( ( #2152, #748, #6508 ) ) REPRESENTATION_CONTEXT ( 'NONE', 'WORKASPACE' ) );
#2799 = CARTESIAN_POINT ( 'NONE',  ( -3.807688866302469071E-16, -29.89062499965859843, -6.218427825808274356 ) ) ;
#2800 = CARTESIAN_POINT ( 'NONE',  ( -2.815599370228907272, -3.150659073900639040, 2.841254879263473754 ) ) ;
#2801 = CARTESIAN_POINT ( 'NONE',  ( 0.000000000000000000, -28.00000000000000000, 0.000000000000000000 ) ) ;
#2802 = DIRECTION ( 'NONE',  ( 0.000000000000000000, 1.000000000000000000, 0.000000000000000000 ) ) ;
#2803 = EDGE_LOOP ( 'NONE', ( #4036, #3583 ) ) ;
#2804 =( NAMED_UNIT ( * ) PLANE_ANGLE_UNIT ( ) SI_UNIT ( $, .RADIAN. ) );
#2805 = CARTESIAN_POINT ( 'NONE',  ( 5.250000000000000000, -29.87500000000000000, -6.429395695523604153E-16 ) ) ;
#2806 = ORIENTED_EDGE ( 'NONE', *, *, #8722, .T. ) ;
#2807 = CARTESIAN_POINT ( 'NONE',  ( 2.557341765624996821, -27.90104166700806587, 4.429445870380401828 ) ) ;
#2808 = CARTESIAN_POINT ( 'NONE',  ( -2.992485675378564469, -3.050659073900639839, 1.260781871532430820 ) ) ;
#2809 = CARTESIAN_POINT ( 'NONE',  ( -5.250000000000000888, -28.85416666666666785, 3.031088913245532979 ) ) ;
#2810 = CARTESIAN_POINT ( 'NONE',  ( 1.000000000000000000, -35.00000000000000000, 2.880243826144208708 ) ) ;
#2811 = CARTESIAN_POINT ( 'NONE',  ( -5.114683531250000748, -28.54687500034139802, -6.263680815196995234E-16 ) ) ;
#2812 = AXIS2_PLACEMENT_3D ( 'NONE', #2836, #8503, #4950 ) ;
#2813 = AXIS2_PLACEMENT_3D ( 'NONE', #5574, #8419, #3666 ) ;
#2814 = CARTESIAN_POINT ( 'NONE',  ( 5.114683531249998971, -27.69270833367472662, 2.952963913586936329 ) ) ;
#2815 = CARTESIAN_POINT ( 'NONE',  ( 6.972266317189433020E-16, -28.46875000068279959, -5.250000000000000000 ) ) ;
#2816 = CARTESIAN_POINT ( 'NONE',  ( -2.624999999999996891, -29.39583333265053611, 4.546633369868304797 ) ) ;
#2817 = CARTESIAN_POINT ( 'NONE',  ( 2.625000000000002220, -27.60416666598386826, 4.546633369868302132 ) ) ;
#2818 = SURFACE_STYLE_USAGE ( .BOTH. , #8439 ) ;
#2819 = CARTESIAN_POINT ( 'NONE',  ( -5.249999999999999112, -27.20833333265053611, -3.031088913245534755 ) ) ;
#2820 = CARTESIAN_POINT ( 'NONE',  ( -0.01814118441321365544, -5.449340926099361937, 3.500000000000000000 ) ) ;
#2821 = SURFACE_STYLE_FILL_AREA ( #1549 ) ;
#2822 = ADVANCED_FACE ( 'NONE', ( #3293 ), #4681, .F. ) ;
#2823 = VERTEX_POINT ( 'NONE', #8221 ) ;
#2824 = VECTOR ( 'NONE', #3809, 1000.000000000000114 ) ;
#2825 = CARTESIAN_POINT ( 'NONE',  ( -2.624999999999996891, -28.89583333265053611, 4.546633369868304797 ) ) ;
#2826 = CARTESIAN_POINT ( 'NONE',  ( -5.114683531250000748, -29.21354166700806587, 2.952963913586931888 ) ) ;
#2827 = EDGE_CURVE ( 'NONE', #4261, #5029, #6109, .T. ) ;
#2828 = ORIENTED_EDGE ( 'NONE', *, *, #6113, .F. ) ;
#2829 = VECTOR ( 'NONE', #7877, 1000.000000000000000 ) ;
#2830 = CARTESIAN_POINT ( 'NONE',  ( 5.385316468749999252, -29.18229166632526983, -3.109213912904138954 ) ) ;
#2831 = CARTESIAN_POINT ( 'NONE',  ( 2.462045979635629767, -7.150659073900639484, -2.487701488670203354 ) ) ;
#2832 = EDGE_CURVE ( 'NONE', #154, #2876, #9188, .T. ) ;
#2833 = AXIS2_PLACEMENT_3D ( 'NONE', #2914, #5731, #2734 ) ;
#2834 = VERTEX_POINT ( 'NONE', #5371 ) ;
#2835 = CARTESIAN_POINT ( 'NONE',  ( -5.250000000000000000, -28.99999999999999645, 0.000000000000000000 ) ) ;
#2836 = CARTESIAN_POINT ( 'NONE',  ( 0.000000000000000000, -28.00000000000000000, 0.000000000000000000 ) ) ;
#2837 = CARTESIAN_POINT ( 'NONE',  ( 0.000000000000000000, 76.00000000000000000, 0.000000000000000000 ) ) ;
#2838 = CARTESIAN_POINT ( 'NONE',  ( 2.557341765624996821, -28.40104166700806587, 4.429445870380401828 ) ) ;
#2839 = CARTESIAN_POINT ( 'NONE',  ( -5.249999999999999112, -28.20833333265053255, -3.031088913245534755 ) ) ;
#2840 = VECTOR ( 'NONE', #2802, 1000.000000000000000 ) ;
#2841 = CARTESIAN_POINT ( 'NONE',  ( -9.180150650966086169E-15, -28.62499999931720396, 5.250000000000000000 ) ) ;
#2842 = CARTESIAN_POINT ( 'NONE',  ( 2.108492589042307408, -7.249340926099360871, 2.134148098076978251 ) ) ;
#2843 = EDGE_CURVE ( 'NONE', #7570, #8796, #8078, .T. ) ;
#2844 = CARTESIAN_POINT ( 'NONE',  ( 6.429395695523604153E-16, -30.00000000000000000, -5.250000000000000000 ) ) ;
#2845 = CARTESIAN_POINT ( 'NONE',  ( 5.385316468750000141, -27.48437499965860198, -6.595110575850215044E-16 ) ) ;
#2846 = CARTESIAN_POINT ( 'NONE',  ( -1.674995433905516196, -1.050659073900638507, -3.992485675378566690 ) ) ;
#2847 = AXIS2_PLACEMENT_3D ( 'NONE', #596, #5567, #4991 ) ;
#2848 = FACE_OUTER_BOUND ( 'NONE', #3562, .T. ) ;
#2849 = CARTESIAN_POINT ( 'NONE',  ( -1.406733260263385521, -26.85491455036743247, 5.250000000000006217 ) ) ;
#2850 = ADVANCED_FACE ( 'NONE', ( #587, #7088 ), #7798, .F. ) ;
#2851 = VERTEX_POINT ( 'NONE', #6956 ) ;
#2852 = SURFACE_SIDE_STYLE ('',( #6497 ) ) ;
#2853 = CARTESIAN_POINT ( 'NONE',  ( -5.250000000000000000, -30.00000000000000000, 0.000000000000000000 ) ) ;
#2854 = EDGE_CURVE ( 'NONE', #7159, #8870, #471, .T. ) ;
#2855 = CARTESIAN_POINT ( 'NONE',  ( 3.616337804771879580E-16, -27.79687500034139802, -5.905927827173866440 ) ) ;
#2856 = CARTESIAN_POINT ( 'NONE',  ( -1.260781871532494103, -6.949340926099362825, 2.992485675378538712 ) ) ;
#2857 = CARTESIAN_POINT ( 'NONE',  ( 5.250000000000000000, -28.97916666666666430, -3.031088913245534755 ) ) ;
#2858 = CARTESIAN_POINT ( 'NONE',  ( 2.624999999999998668, -29.33333333333333215, -4.546633369868303021 ) ) ;
#2859 = CARTESIAN_POINT ( 'NONE',  ( -5.114683531250000748, -28.81770833367473017, -2.952963913586935440 ) ) ;
#2860 = CARTESIAN_POINT ( 'NONE',  ( -1.084901341431563923E-15, -27.48437500034140157, 5.905927827173866440 ) ) ;
#2861 = CARTESIAN_POINT ( 'NONE',  ( 5.250000000000000888, -28.83333333265053611, 3.031088913245532979 ) ) ;
#2862 = CARTESIAN_POINT ( 'NONE',  ( 1.975475456537005874E-15, -27.62499999931720041, 5.250000000000000000 ) ) ;
#2863 = CARTESIAN_POINT ( 'NONE',  ( -2.475000949148032703, -1.535234168964353515E-16, 2.672592990517839606 ) ) ;
#2864 = FACE_OUTER_BOUND ( 'NONE', #22, .T. ) ;
#2865 = CARTESIAN_POINT ( 'NONE',  ( 2.557341765624996821, -29.46354166700806232, 4.429445870380401828 ) ) ;
#2866 = CARTESIAN_POINT ( 'NONE',  ( -3.507514324621464397, -3.549340926099361582, 1.431606283892619347 ) ) ;
#2867 = ORIENTED_EDGE ( 'NONE', *, *, #546, .T. ) ;
#2868 = CARTESIAN_POINT ( 'NONE',  ( 2.939207850660410271E-16, -20.00000000000000000, 2.050090691792606279 ) ) ;
#2869 = CARTESIAN_POINT ( 'NONE',  ( 5.114683531249998971, -29.13020833367473372, 2.952963913586936329 ) ) ;
#2870 = VERTEX_POINT ( 'NONE', #4817 ) ;
#2871 = ORIENTED_EDGE ( 'NONE', *, *, #814, .T. ) ;
#2872 = CARTESIAN_POINT ( 'NONE',  ( -2.692658234375000514, -29.86979166632526983, -4.663820869356205989 ) ) ;
#2873 = CARTESIAN_POINT ( 'NONE',  ( 1.431606283892694842, -7.250659073900640017, -3.507514324621434199 ) ) ;
#2874 = AXIS2_PLACEMENT_3D ( 'NONE', #6008, #1886, #6200 ) ;
#2875 = CARTESIAN_POINT ( 'NONE',  ( -1.406733260263393293, -27.17633545031536713, -5.250000000000000000 ) ) ;
#2876 = VERTEX_POINT ( 'NONE', #1372 ) ;
#2877 = ADVANCED_FACE ( 'NONE', ( #7837 ), #711, .F. ) ;
#2878 = DIRECTION ( 'NONE',  ( 0.000000000000000000, -1.000000000000000000, 0.000000000000000000 ) ) ;
#2879 = VECTOR ( 'NONE', #508, 1000.000000000000000 ) ;
#2880 = FACE_OUTER_BOUND ( 'NONE', #8908, .T. ) ;
#2881 = CARTESIAN_POINT ( 'NONE',  ( -2.033577675846918216E-14, -28.93750000000000000, 5.250000000000000888 ) ) ;
#2882 = MECHANICAL_DESIGN_GEOMETRIC_PRESENTATION_REPRESENTATION (  '', ( #1097 ), #1531 ) ;
#2883 = CARTESIAN_POINT ( 'NONE',  ( -2.557341765624999042, -28.77604166700806587, -4.429445870380400052 ) ) ;
#2884 = CARTESIAN_POINT ( 'NONE',  ( 5.250000000000000000, -27.53125000068279604, 0.000000000000000000 ) ) ;
#2885 = CONTEXT_DEPENDENT_SHAPE_REPRESENTATION ( #8949, #7575 ) ;
#2886 = CARTESIAN_POINT ( 'NONE',  ( -1.406733260263387963, -28.95758545099816672, -5.250000000000001776 ) ) ;
#2887 = CARTESIAN_POINT ( 'NONE',  ( -3.000000000000000444, -3.449340926099361493, -0.01814118441320822922 ) ) ;
#2888 = CARTESIAN_POINT ( 'NONE',  ( -1.406733260263382856, -28.20758545099816317, -5.250000000000006217 ) ) ;
#2889 = CARTESIAN_POINT ( 'NONE',  ( -2.692658234375000514, -28.15104166632526628, -4.663820869356205989 ) ) ;
#2890 = CARTESIAN_POINT ( 'NONE',  ( -1.674995433905516196, -2.650659073900639040, -3.992485675378566690 ) ) ;
#2891 = CIRCLE ( 'NONE', #647, 1.499999999999999778 ) ;
#2892 = CARTESIAN_POINT ( 'NONE',  ( 2.625000000000000444, -27.20833333333333215, -4.546633369868303021 ) ) ;
#2893 = DIRECTION ( 'NONE',  ( -8.881784197001252323E-16, 0.000000000000000000, -1.000000000000000000 ) ) ;
#2894 = ORIENTED_EDGE ( 'NONE', *, *, #1762, .T. ) ;
#2895 = CARTESIAN_POINT ( 'NONE',  ( 5.385316468750001029, -27.47395833299193413, 3.109213912904135846 ) ) ;
#2896 = EDGE_LOOP ( 'NONE', ( #2606, #5966, #5717, #4939 ) ) ;
#2897 = CARTESIAN_POINT ( 'NONE',  ( 2.557341765624996821, -26.90104166700806232, 4.429445870380401828 ) ) ;
#2898 = CARTESIAN_POINT ( 'NONE',  ( 2.134148098076933397, -1.950659073900639306, 2.108492589042352261 ) ) ;
#2899 = ORIENTED_EDGE ( 'NONE', *, *, #1197, .T. ) ;
#2900 = CARTESIAN_POINT ( 'NONE',  ( -1.113604000661152470E-15, -29.56250000000000000, 6.062177826491070398 ) ) ;
#2901 = PLANE ( 'NONE',  #5691 ) ;
#2902 =( BOUNDED_CURVE ( )  B_SPLINE_CURVE ( 2, ( #7900, #7945, #1519, #4364, #821, #863, #3712, #2407, #6537, #170, #3020, #2315, #7335, #8032, #3761, #5190, #5141, #7984, #1663, #1612, #4450, #7289, #961, #914, #6590, #4504, #8862, #3249, #4043, #4639, #8179, #7620, #3391, #2649, #1860, #2607, #1058, #1808, #3901, #7477, #6220, #1247, #9050, #8271, #6722, #4730, #354, #3346, #8956, #452, #4778, #1107, #4685, #6125, #548, #1902, #401, #1151, #2502, #6025, #6072, #4594, #4087, #8909, #8318, #7572, #9003, #1201, #6875, #5423, #503, #2556, #6922, #6176, #5471, #5283, #1948, #3947, #8227, #8130, #3206, #1758, #6774, #7432, #5326, #5376, #7522, #3994, #6827, #3298, #1287, #2119, #2784, #592, #4258, #4127, #1375, #5604, #2076, #4821, #8408, #2830, #6961, #674, #4173, #7092, #9139, #4985, #6264, #3435, #8449, #1459, #7706, #632, #4902, #9095, #5649, #3476, #5521, #2035, #7842, #5693, #8538, #6344, #3518, #2743, #765, #6303, #5563, #3607, #1418, #7753, #7665, #4306, #2872, #716, #4858, #7801, #9178, #3564, #1331, #7142, #7007, #4945, #4218 ),
 .UNSPECIFIED., .F., .F. ) 
 B_SPLINE_CURVE_WITH_KNOTS ( ( 3, 2, 2, 2, 2, 2, 2, 2, 2, 2, 2, 2, 2, 2, 2, 2, 2, 2, 2, 2, 2, 2, 2, 2, 2, 2, 2, 2, 2, 2, 2, 2, 2, 2, 2, 2, 2, 2, 2, 2, 2, 2, 2, 2, 2, 2, 2, 2, 2, 2, 2, 2, 2, 2, 2, 2, 2, 2, 2, 2, 2, 2, 2, 2, 2, 2, 2, 2, 2, 2, 2, 2, 3 ),
 ( 0.000000000000000000, 0.01388888888888888812, 0.02777777777777777624, 0.04166666666666666435, 0.05555555555555555247, 0.06944444444444444753, 0.08333333333333332871, 0.09722222222222222376, 0.1111111111111111049, 0.1250000000000000000, 0.1388888888888888951, 0.1527777777777777901, 0.1666666666666666574, 0.1805555555555555525, 0.1944444444444444475, 0.2083333333333333426, 0.2222222222222222099, 0.2361111111111111049, 0.2500000000000000000, 0.2638888888888888951, 0.2777777777777777901, 0.2916666666666666852, 0.3055555555555555802, 0.3194444444444444198, 0.3333333333333333148, 0.3472222222222222099, 0.3611111111111111049, 0.3750000000000000000, 0.3888888888888888951, 0.4027777777777777901, 0.4166666666666666852, 0.4305555555555555802, 0.4444444444444444198, 0.4583333333333333148, 0.4722222222222222099, 0.4861111111111111049, 0.5000000000000000000, 0.5138888888888888395, 0.5277777777777777901, 0.5416666666666666297, 0.5555555555555555802, 0.5694444444444444198, 0.5833333333333333703, 0.5972222222222222099, 0.6111111111111111605, 0.6250000000000000000, 0.6388888888888888395, 0.6527777777777777901, 0.6666666666666666297, 0.6805555555555555802, 0.6944444444444444198, 0.7083333333333333703, 0.7222222222222222099, 0.7361111111111111605, 0.7500000000000000000, 0.7638888888888888395, 0.7777777777777777901, 0.7916666666666666297, 0.8055555555555555802, 0.8194444444444444198, 0.8333333333333333703, 0.8472222222222222099, 0.8611111111111111605, 0.8750000000000000000, 0.8888888888888888395, 0.9027777777777777901, 0.9166666666666666297, 0.9305555555555555802, 0.9444444444444444198, 0.9583333333333333703, 0.9722222222222222099, 0.9861111111111111605, 1.000000000000000000 ),
 .UNSPECIFIED. ) 
 CURVE ( )  GEOMETRIC_REPRESENTATION_ITEM ( )  RATIONAL_B_SPLINE_CURVE ( ( 1.000000000000000000, 0.8660254037844387076, 1.000000000000000000, 0.8660254037844387076, 1.000000000000000000, 0.8660254037844387076, 1.000000000000000000, 0.8660254037844387076, 1.000000000000000000, 0.8660254037844387076, 1.000000000000000000, 0.8660254037844387076, 1.000000000000000000, 0.8660254037844387076, 1.000000000000000000, 0.8660254037844387076, 1.000000000000000000, 0.8660254037844387076, 1.000000000000000000, 0.8660254037844387076, 1.000000000000000000, 0.8660254037844387076, 1.000000000000000000, 0.8660254037844387076, 1.000000000000000000, 0.8660254037844387076, 1.000000000000000000, 0.8660254037844387076, 1.000000000000000000, 0.8660254037844387076, 1.000000000000000000, 0.8660254037844387076, 1.000000000000000000, 0.8660254037844387076, 1.000000000000000000, 0.8660254037844387076, 1.000000000000000000, 0.8660254037844387076, 1.000000000000000000, 0.8660254037844387076, 1.000000000000000000, 0.8660254037844387076, 1.000000000000000000, 0.8660254037844387076, 1.000000000000000000, 0.8660254037844387076, 1.000000000000000000, 0.8660254037844387076, 1.000000000000000000, 0.8660254037844387076, 1.000000000000000000, 0.8660254037844387076, 1.000000000000000000, 0.8660254037844387076, 1.000000000000000000, 0.8660254037844387076, 1.000000000000000000, 0.8660254037844387076, 1.000000000000000000, 0.8660254037844387076, 1.000000000000000000, 0.8660254037844387076, 1.000000000000000000, 0.8660254037844387076, 1.000000000000000000, 0.8660254037844387076, 1.000000000000000000, 0.8660254037844387076, 1.000000000000000000, 0.8660254037844387076, 1.000000000000000000, 0.8660254037844387076, 1.000000000000000000, 0.8660254037844387076, 1.000000000000000000, 0.8660254037844387076, 1.000000000000000000, 0.8660254037844387076, 1.000000000000000000, 0.8660254037844387076, 1.000000000000000000, 0.8660254037844387076, 1.000000000000000000, 0.8660254037844387076, 1.000000000000000000, 0.8660254037844387076, 1.000000000000000000, 0.8660254037844387076, 1.000000000000000000, 0.8660254037844387076, 1.000000000000000000, 0.8660254037844387076, 1.000000000000000000, 0.8660254037844387076, 1.000000000000000000, 0.8660254037844387076, 1.000000000000000000, 0.8660254037844387076, 1.000000000000000000, 0.8660254037844387076, 1.000000000000000000, 0.8660254037844387076, 1.000000000000000000, 0.8660254037844387076, 1.000000000000000000, 0.8660254037844387076, 1.000000000000000000, 0.8660254037844387076, 1.000000000000000000, 0.8660254037844387076, 1.000000000000000000, 0.8660254037844387076, 1.000000000000000000, 0.8660254037844387076, 1.000000000000000000, 0.8660254037844387076, 1.000000000000000000, 0.8660254037844387076, 1.000000000000000000, 0.8660254037844387076, 1.000000000000000000, 0.8660254037844387076, 1.000000000000000000, 0.8660254037844387076, 1.000000000000000000, 0.8660254037844387076, 1.000000000000000000, 0.8660254037844387076, 1.000000000000000000, 0.8660254037844387076, 1.000000000000000000, 0.8660254037844387076, 1.000000000000000000, 0.8660254037844387076, 1.000000000000000000, 0.8660254037844387076, 1.000000000000000000, 0.8660254037844387076, 1.000000000000000000, 0.8660254037844387076, 1.000000000000000000, 0.8660254037844387076, 1.000000000000000000, 0.8660254037844387076, 1.000000000000000000 ) ) 
 REPRESENTATION_ITEM ( '' )  );
#2903 = CARTESIAN_POINT ( 'NONE',  ( -2.557341765625002594, -27.75520833367473017, 4.429445870380399164 ) ) ;
#2904 = APPLICATION_CONTEXT ( 'automotive_design' ) ;
#2905 = CARTESIAN_POINT ( 'NONE',  ( 2.557341765625000818, -27.63020833367473017, -4.429445870380400052 ) ) ;
#2906 = FACE_OUTER_BOUND ( 'NONE', #4988, .T. ) ;
#2907 = CYLINDRICAL_SURFACE ( 'NONE', #7179, 2.500000000000000000 ) ;
#2908 = CARTESIAN_POINT ( 'NONE',  ( 0.000000000000000000, -9.000000000000000000, 0.000000000000000000 ) ) ;
#2909 = FACE_OUTER_BOUND ( 'NONE', #4484, .T. ) ;
#2910 = CARTESIAN_POINT ( 'NONE',  ( -3.492485675378536047, -8.149340926099361226, -1.467888652719048670 ) ) ;
#2911 = CARTESIAN_POINT ( 'NONE',  ( 1.431606283892619125, -7.149340926099362115, 3.507514324621464397 ) ) ;
#2912 = ORIENTED_EDGE ( 'NONE', *, *, #3174, .T. ) ;
#2913 = CARTESIAN_POINT ( 'NONE',  ( -3.507514324621433754, -6.050659073900638951, -1.431606283892695064 ) ) ;
#2914 = CARTESIAN_POINT ( 'NONE',  ( 0.000000000000000000, -27.00000000000000000, 0.000000000000000000 ) ) ;
#2915 = CARTESIAN_POINT ( 'NONE',  ( -2.557341765625002594, -29.69270833367473017, 4.429445870380399164 ) ) ;
#2916 = ORIENTED_EDGE ( 'NONE', *, *, #924, .F. ) ;
#2917 = EDGE_CURVE ( 'NONE', #1598, #6037, #1326, .T. ) ;
#2918 = ORIENTED_EDGE ( 'NONE', *, *, #7856, .F. ) ;
#2919 = CARTESIAN_POINT ( 'NONE',  ( 2.624999999999998668, -29.58333333333333215, -4.546633369868303021 ) ) ;
#2920 = CARTESIAN_POINT ( 'NONE',  ( 2.841254879263473310, -0.3506590739006385515, 2.815599370228907272 ) ) ;
#2921 = LINE ( 'NONE', #5738, #5025 ) ;
#2922 = ORIENTED_EDGE ( 'NONE', *, *, #5548, .F. ) ;
#2923 = CARTESIAN_POINT ( 'NONE',  ( 2.300847884672513123E-14, -27.68750000000000000, -5.250000000000000000 ) ) ;
#2924 = LINE ( 'NONE', #1514, #574 ) ;
#2925 = CARTESIAN_POINT ( 'NONE',  ( 1.000000000000000000, -35.00000000000000000, -3.048902179152658931 ) ) ;
#2926 = CARTESIAN_POINT ( 'NONE',  ( -5.114683531249999859, -27.00520833367473017, -2.952963913586935440 ) ) ;
#2927 = DIRECTION ( 'NONE',  ( 0.000000000000000000, -1.000000000000000000, 0.000000000000000000 ) ) ;
#2928 = CARTESIAN_POINT ( 'NONE',  ( 3.061616997868383634E-16, 0.000000000000000000, -2.500000000000000444 ) ) ;
#2929 = CARTESIAN_POINT ( 'NONE',  ( 0.01814118441320878086, -6.249340926099361759, -3.000000000000000444 ) ) ;
#2930 = DIRECTION ( 'NONE',  ( 0.000000000000000000, -1.000000000000000000, 0.000000000000000000 ) ) ;
#2931 = CARTESIAN_POINT ( 'NONE',  ( 1.142306659890740623E-15, -28.29687499965860553, 6.218427825808274356 ) ) ;
#2932 = CARTESIAN_POINT ( 'NONE',  ( 4.007514324621469726, -2.749340926099360427, -1.638713065079161257 ) ) ;
#2933 = CARTESIAN_POINT ( 'NONE',  ( 1.000000000000000000, -35.00000000000000000, 1.118033988749894680 ) ) ;
#2934 = CARTESIAN_POINT ( 'NONE',  ( 4.286263797015737088E-16, -20.00000000000000000, 3.500000000000000444 ) ) ;
#2935 = PRODUCT_DEFINITION_SHAPE ( 'NONE', 'NONE',  #349 ) ;
#2936 = VERTEX_POINT ( 'NONE', #2868 ) ;
#2937 = CARTESIAN_POINT ( 'NONE',  ( 1.142306659890740623E-15, -27.26562499965860553, 6.218427825808274356 ) ) ;
#2938 = EDGE_LOOP ( 'NONE', ( #2622, #8965, #3970, #2477 ) ) ;
#2939 = DIRECTION ( 'NONE',  ( 0.000000000000000000, -1.000000000000000000, 0.000000000000000000 ) ) ;
#2940 = CARTESIAN_POINT ( 'NONE',  ( -3.500000000000000000, -1.350659073900638996, 0.01814118441314012051 ) ) ;
#2941 = ORIENTED_EDGE ( 'NONE', *, *, #7646, .F. ) ;
#2942 = CARTESIAN_POINT ( 'NONE',  ( -1.113604000661152470E-15, -28.56249999999999645, 6.062177826491070398 ) ) ;
#2943 =( NAMED_UNIT ( * ) SI_UNIT ( $, .STERADIAN. ) SOLID_ANGLE_UNIT ( ) );
#2944 = EDGE_CURVE ( 'NONE', #4857, #7379, #5220, .T. ) ;
#2945 = PRODUCT_DEFINITION_FORMATION_WITH_SPECIFIED_SOURCE ( 'ANY', '', #8393, .NOT_KNOWN. ) ;
#2946 = CARTESIAN_POINT ( 'NONE',  ( 5.114683531250000748, -28.17187500034139447, 0.000000000000000000 ) ) ;
#2947 = CARTESIAN_POINT ( 'NONE',  ( -5.114683531250000748, -28.02604166700806587, 2.952963913586931888 ) ) ;
#2948 = MECHANICAL_DESIGN_GEOMETRIC_PRESENTATION_REPRESENTATION (  '', ( #5632 ), #3563 ) ;
#2949 = DIRECTION ( 'NONE',  ( -0.000000000000000000, -1.000000000000000000, -0.000000000000000000 ) ) ;
#2950 =( BOUNDED_SURFACE ( )  B_SPLINE_SURFACE ( 3, 2, ( 
 ( #1319, #6996, #622, #3464, #5216, #5913, #2436, #1640, #4528, #3142, #3829, #195, #7216, #4477, #5262, #2244, #7315, #8800, #285, #1545, #5866, #1736, #6703, #2386, #840, #8058, #4386, #6655, #3090, #7359, #6611, #983, #940, #3048, #892, #240, #8706, #5962, #7920, #5067, #2336, #3687, #1688, #8755, #8107, #3788, #4572, #7408, #1031, #5167, #6512, #3881, #332, #149, #3185, #8613, #2999, #5821, #8009, #8660, #2292, #5117, #7964, #1589, #4429, #7264, #3742, #6563, #477, #6199, #527, #6854, #1270, #2631, #1132, #1885, #380, #6754, #6801, #2582, #3368 ),
 ( #3273, #8203, #4619, #426, #569, #2673, #2529, #9027, #7458, #4756, #3926, #5498, #8345, #5306, #1833, #4665, #5402, #1970, #3229, #6940, #5450, #6154, #4710, #1928, #4799, #2482, #8888, #1176, #8252, #7504, #5354, #3972, #6050, #8295, #4019, #1785, #7642, #6103, #7600, #1224, #4064, #7549, #6006, #8933, #3323, #4108, #8845, #1084, #8982, #6903, #8157, #4241, #2765, #7031, #2015, #2718, #4840, #5716, #4151, #7072, #696, #614, #1486, #1357, #3455, #4330, #2147, #2856, #4968, #3541, #658, #2102, #7822, #4925, #4196, #4882, #1400, #3500, #1438, #5543, #9076 ),
 ( #6366, #6411, #5628, #8520, #7117, #4284, #6323, #7685, #8477, #50, #6242, #7778, #3587, #740, #8388, #9159, #8559, #7163, #5, #1309, #5672, #6986, #2898, #2187, #5009, #7865, #3413, #6284, #9120, #5585, #8429, #7733, #2057, #2808, #1534, #1582, #6555, #7350, #7912, #5813, #4563, #7255, #2989, #8603, #4423, #790, #6647, #6501, #4521, #2234, #8744, #4377, #276, #976, #90, #8651, #2283, #185, #3130, #7209, #1726, #234, #929, #5859, #5905, #5953, #6456, #3679, #5159, #3040, #5109, #138, #7958, #834, #3083, #8001, #5761, #8792, #882, #2378, #5207 ),
 ( #8699, #3731, #5059, #2423, #2330, #1630, #4468, #7306, #3779, #6605, #3634, #8049, #1677, #3822, #5253, #8098, #2940, #6190, #4610, #3311, #7398, #3219, #2664, #2472, #6842, #6143, #7538, #4652, #6090, #8971, #2621, #6039, #5438, #8876, #1875, #8284, #2517, #5486, #518, #1918, #8334, #1964, #466, #4742, #5343, #8192, #1774, #1821, #7589, #6741, #1073, #3360, #1021, #1215, #3962, #4699, #3175, #3916, #5997, #371, #3871, #4055, #1164, #6692, #8147, #7495, #5296, #1121, #322, #9018, #7448, #6890, #6788, #414, #4008, #8836, #3262, #8923, #2573, #5390, #8241 ),
 ( #8421, #7814, #7767, #8511, #1390, #3534, #4919, #5619, #2756, #9067, #4143, #731, #1431, #2846, #1301, #7721, #4234, #2008, #5707, #7108, #7064, #6404, #4276, #9152, #3449, #3579, #562, #40, #688, #2890, #6976, #6358, #6316, #6276, #2800, #1349, #3491, #6235, #7634, #9111, #8466, #2094, #5577, #3401, #2049, #646, #7020, #4874, #3406, #8551, #605, #4187, #5665, #5536, #2137, #4959, #1262, #4790, #2708, #4102, #6934, #8379, #4833, #7679, #8594, #7293, #2179, #7201, #6767, #6448, #1616, #917, #2318, #8639, #866, #3765, #1523, #5801, #779, #1477, #3626 ),
 ( #3024, #2224, #395, #127, #5049, #3242, #6593, #1570, #7156, #4507, #2364, #223, #82, #3072, #174, #5893, #3716, #2976, #3668, #5847, #2270, #8733, #4320, #7857, #5098, #2932, #7987, #8687, #5194, #4411, #8036, #1666, #7338, #7948, #5753, #7242, #1100, #5000, #6542, #3940, #6066, #7904, #5146, #4367, #825, #4454, #6493, #8358, #4679, #6954, #3381, #4770, #6214, #9089, #3428, #540, #4166, #5515, #4035, #7614, #3290, #444, #493, #5464, #6257, #6817, #4723, #3468, #6169, #1896, #7516, #3340, #8901, #5557, #5416, #2730, #1145, #7659, #6118, #8401, #2029 ),
 ( #4852, #1983, #1323, #7698, #4080, #7564, #7000, #3988, #626, #4814, #2546, #8265, #2687, #1238, #1192, #6916, #2643, #9043, #8947, #5369, #6869, #1281, #4120, #8995, #584, #8310, #8218, #1942, #1852, #2599, #5072, #2113, #4253, #2866, #7044, #62, #708, #4895, #5598, #7746, #8617, #668, #755, #7134, #3513, #4390, #7086, #6336, #7219, #5023, #5685, #2067, #2248, #6469, #4342, #4210, #2201, #4296, #7880, #7835, #3556, #7796, #3600, #6378, #1500, #8442, #2777, #18, #1370, #2911, #6425, #104, #8531, #7178, #802, #3646, #2159, #9173, #4979, #2955, #9133 ) ),
 .UNSPECIFIED., .T., .F., .T. ) 
 B_SPLINE_SURFACE_WITH_KNOTS ( ( 4, 3, 4 ),
 ( 3, 2, 2, 2, 2, 2, 2, 2, 2, 2, 2, 2, 2, 2, 2, 2, 2, 2, 2, 2, 2, 2, 2, 2, 2, 2, 2, 2, 2, 2, 2, 2, 2, 2, 2, 2, 2, 2, 2, 2, 3 ),
 ( 0.000000000000000000, 0.5000000000000000000, 1.000000000000000000 ),
 ( 0.000000000000000000, 0.02500000000000000139, 0.05000000000000000278, 0.07499999999999999722, 0.1000000000000000056, 0.1250000000000000000, 0.1499999999999999944, 0.1749999999999999889, 0.2000000000000000111, 0.2250000000000000056, 0.2500000000000000000, 0.2750000000000000222, 0.2999999999999999889, 0.3250000000000000111, 0.3499999999999999778, 0.3750000000000000000, 0.4000000000000000222, 0.4249999999999999889, 0.4500000000000000111, 0.4749999999999999778, 0.5000000000000000000, 0.5250000000000000222, 0.5500000000000000444, 0.5749999999999999556, 0.5999999999999999778, 0.6250000000000000000, 0.6500000000000000222, 0.6750000000000000444, 0.6999999999999999556, 0.7249999999999999778, 0.7500000000000000000, 0.7750000000000000222, 0.8000000000000000444, 0.8249999999999999556, 0.8499999999999999778, 0.8750000000000000000, 0.9000000000000000222, 0.9250000000000000444, 0.9499999999999999556, 0.9749999999999999778, 1.000000000000000000 ),
 .UNSPECIFIED. ) 
 GEOMETRIC_REPRESENTATION_ITEM ( )  RATIONAL_B_SPLINE_SURFACE ( (
 ( 1.000000000000000000, 0.9238795325112867385, 1.000000000000000000, 0.9238795325112867385, 1.000000000000000000, 0.9238795325112867385, 1.000000000000000000, 0.9238795325112867385, 1.000000000000000000, 0.9238795325112867385, 1.000000000000000000, 0.9238795325112867385, 1.000000000000000000, 0.9238795325112867385, 1.000000000000000000, 0.9238795325112867385, 1.000000000000000000, 0.9238795325112867385, 1.000000000000000000, 0.9238795325112867385, 1.000000000000000000, 0.9238795325112867385, 1.000000000000000000, 0.9238795325112867385, 1.000000000000000000, 0.9238795325112867385, 1.000000000000000000, 0.9238795325112867385, 1.000000000000000000, 0.9238795325112867385, 1.000000000000000000, 0.9238795325112867385, 1.000000000000000000, 0.9238795325112867385, 1.000000000000000000, 0.9238795325112867385, 1.000000000000000000, 0.9238795325112867385, 1.000000000000000000, 0.9238795325112867385, 1.000000000000000000, 0.9238795325112867385, 1.000000000000000000, 0.9238795325112867385, 1.000000000000000000, 0.9238795325112867385, 1.000000000000000000, 0.9238795325112867385, 1.000000000000000000, 0.9238795325112867385, 1.000000000000000000, 0.9238795325112867385, 1.000000000000000000, 0.9238795325112867385, 1.000000000000000000, 0.9238795325112867385, 1.000000000000000000, 0.9238795325112867385, 1.000000000000000000, 0.9238795325112867385, 1.000000000000000000, 0.9238795325112867385, 1.000000000000000000, 0.9238795325112867385, 1.000000000000000000, 0.9238795325112867385, 1.000000000000000000, 0.9238795325112867385, 1.000000000000000000, 0.9238795325112867385, 1.000000000000000000, 0.9238795325112867385, 1.000000000000000000, 0.9238795325112867385, 1.000000000000000000, 0.9238795325112867385, 1.000000000000000000, 0.9238795325112867385, 1.000000000000000000, 0.9238795325112867385, 1.000000000000000000),
 ( 0.3333333333333333703, 0.3079598441704289313, 0.3333333333333333703, 0.3079598441704289313, 0.3333333333333333703, 0.3079598441704289313, 0.3333333333333333703, 0.3079598441704289313, 0.3333333333333333703, 0.3079598441704289313, 0.3333333333333333703, 0.3079598441704289313, 0.3333333333333333703, 0.3079598441704289313, 0.3333333333333333703, 0.3079598441704289313, 0.3333333333333333703, 0.3079598441704289313, 0.3333333333333333703, 0.3079598441704289313, 0.3333333333333333703, 0.3079598441704289313, 0.3333333333333333703, 0.3079598441704289313, 0.3333333333333333703, 0.3079598441704289313, 0.3333333333333333703, 0.3079598441704289313, 0.3333333333333333703, 0.3079598441704289313, 0.3333333333333333703, 0.3079598441704289313, 0.3333333333333333703, 0.3079598441704289313, 0.3333333333333333703, 0.3079598441704289313, 0.3333333333333333703, 0.3079598441704289313, 0.3333333333333333703, 0.3079598441704289313, 0.3333333333333333703, 0.3079598441704289313, 0.3333333333333333703, 0.3079598441704289313, 0.3333333333333333703, 0.3079598441704289313, 0.3333333333333333703, 0.3079598441704289313, 0.3333333333333333703, 0.3079598441704289313, 0.3333333333333333703, 0.3079598441704289313, 0.3333333333333333703, 0.3079598441704289313, 0.3333333333333333703, 0.3079598441704289313, 0.3333333333333333703, 0.3079598441704289313, 0.3333333333333333703, 0.3079598441704289313, 0.3333333333333333703, 0.3079598441704289313, 0.3333333333333333703, 0.3079598441704289313, 0.3333333333333333703, 0.3079598441704289313, 0.3333333333333333703, 0.3079598441704289313, 0.3333333333333333703, 0.3079598441704289313, 0.3333333333333333703, 0.3079598441704289313, 0.3333333333333333703, 0.3079598441704289313, 0.3333333333333333703, 0.3079598441704289313, 0.3333333333333333703, 0.3079598441704289313, 0.3333333333333333703, 0.3079598441704289313, 0.3333333333333333703),
 ( 0.3333333333333333703, 0.3079598441704289313, 0.3333333333333333703, 0.3079598441704289313, 0.3333333333333333703, 0.3079598441704289313, 0.3333333333333333703, 0.3079598441704289313, 0.3333333333333333703, 0.3079598441704289313, 0.3333333333333333703, 0.3079598441704289313, 0.3333333333333333703, 0.3079598441704289313, 0.3333333333333333703, 0.3079598441704289313, 0.3333333333333333703, 0.3079598441704289313, 0.3333333333333333703, 0.3079598441704289313, 0.3333333333333333703, 0.3079598441704289313, 0.3333333333333333703, 0.3079598441704289313, 0.3333333333333333703, 0.3079598441704289313, 0.3333333333333333703, 0.3079598441704289313, 0.3333333333333333703, 0.3079598441704289313, 0.3333333333333333703, 0.3079598441704289313, 0.3333333333333333703, 0.3079598441704289313, 0.3333333333333333703, 0.3079598441704289313, 0.3333333333333333703, 0.3079598441704289313, 0.3333333333333333703, 0.3079598441704289313, 0.3333333333333333703, 0.3079598441704289313, 0.3333333333333333703, 0.3079598441704289313, 0.3333333333333333703, 0.3079598441704289313, 0.3333333333333333703, 0.3079598441704289313, 0.3333333333333333703, 0.3079598441704289313, 0.3333333333333333703, 0.3079598441704289313, 0.3333333333333333703, 0.3079598441704289313, 0.3333333333333333703, 0.3079598441704289313, 0.3333333333333333703, 0.3079598441704289313, 0.3333333333333333703, 0.3079598441704289313, 0.3333333333333333703, 0.3079598441704289313, 0.3333333333333333703, 0.3079598441704289313, 0.3333333333333333703, 0.3079598441704289313, 0.3333333333333333703, 0.3079598441704289313, 0.3333333333333333703, 0.3079598441704289313, 0.3333333333333333703, 0.3079598441704289313, 0.3333333333333333703, 0.3079598441704289313, 0.3333333333333333703, 0.3079598441704289313, 0.3333333333333333703, 0.3079598441704289313, 0.3333333333333333703, 0.3079598441704289313, 0.3333333333333333703),
 ( 1.000000000000000000, 0.9238795325112867385, 1.000000000000000000, 0.9238795325112867385, 1.000000000000000000, 0.9238795325112867385, 1.000000000000000000, 0.9238795325112867385, 1.000000000000000000, 0.9238795325112867385, 1.000000000000000000, 0.9238795325112867385, 1.000000000000000000, 0.9238795325112867385, 1.000000000000000000, 0.9238795325112867385, 1.000000000000000000, 0.9238795325112867385, 1.000000000000000000, 0.9238795325112867385, 1.000000000000000000, 0.9238795325112867385, 1.000000000000000000, 0.9238795325112867385, 1.000000000000000000, 0.9238795325112867385, 1.000000000000000000, 0.9238795325112867385, 1.000000000000000000, 0.9238795325112867385, 1.000000000000000000, 0.9238795325112867385, 1.000000000000000000, 0.9238795325112867385, 1.000000000000000000, 0.9238795325112867385, 1.000000000000000000, 0.9238795325112867385, 1.000000000000000000, 0.9238795325112867385, 1.000000000000000000, 0.9238795325112867385, 1.000000000000000000, 0.9238795325112867385, 1.000000000000000000, 0.9238795325112867385, 1.000000000000000000, 0.9238795325112867385, 1.000000000000000000, 0.9238795325112867385, 1.000000000000000000, 0.9238795325112867385, 1.000000000000000000, 0.9238795325112867385, 1.000000000000000000, 0.9238795325112867385, 1.000000000000000000, 0.9238795325112867385, 1.000000000000000000, 0.9238795325112867385, 1.000000000000000000, 0.9238795325112867385, 1.000000000000000000, 0.9238795325112867385, 1.000000000000000000, 0.9238795325112867385, 1.000000000000000000, 0.9238795325112867385, 1.000000000000000000, 0.9238795325112867385, 1.000000000000000000, 0.9238795325112867385, 1.000000000000000000, 0.9238795325112867385, 1.000000000000000000, 0.9238795325112867385, 1.000000000000000000, 0.9238795325112867385, 1.000000000000000000, 0.9238795325112867385, 1.000000000000000000),
 ( 0.3333333333333333703, 0.3079598441704289313, 0.3333333333333333703, 0.3079598441704289313, 0.3333333333333333703, 0.3079598441704289313, 0.3333333333333333703, 0.3079598441704289313, 0.3333333333333333703, 0.3079598441704289313, 0.3333333333333333703, 0.3079598441704289313, 0.3333333333333333703, 0.3079598441704289313, 0.3333333333333333703, 0.3079598441704289313, 0.3333333333333333703, 0.3079598441704289313, 0.3333333333333333703, 0.3079598441704289313, 0.3333333333333333703, 0.3079598441704289313, 0.3333333333333333703, 0.3079598441704289313, 0.3333333333333333703, 0.3079598441704289313, 0.3333333333333333703, 0.3079598441704289313, 0.3333333333333333703, 0.3079598441704289313, 0.3333333333333333703, 0.3079598441704289313, 0.3333333333333333703, 0.3079598441704289313, 0.3333333333333333703, 0.3079598441704289313, 0.3333333333333333703, 0.3079598441704289313, 0.3333333333333333703, 0.3079598441704289313, 0.3333333333333333703, 0.3079598441704289313, 0.3333333333333333703, 0.3079598441704289313, 0.3333333333333333703, 0.3079598441704289313, 0.3333333333333333703, 0.3079598441704289313, 0.3333333333333333703, 0.3079598441704289313, 0.3333333333333333703, 0.3079598441704289313, 0.3333333333333333703, 0.3079598441704289313, 0.3333333333333333703, 0.3079598441704289313, 0.3333333333333333703, 0.3079598441704289313, 0.3333333333333333703, 0.3079598441704289313, 0.3333333333333333703, 0.3079598441704289313, 0.3333333333333333703, 0.3079598441704289313, 0.3333333333333333703, 0.3079598441704289313, 0.3333333333333333703, 0.3079598441704289313, 0.3333333333333333703, 0.3079598441704289313, 0.3333333333333333703, 0.3079598441704289313, 0.3333333333333333703, 0.3079598441704289313, 0.3333333333333333703, 0.3079598441704289313, 0.3333333333333333703, 0.3079598441704289313, 0.3333333333333333703, 0.3079598441704289313, 0.3333333333333333703),
 ( 0.3333333333333333703, 0.3079598441704289313, 0.3333333333333333703, 0.3079598441704289313, 0.3333333333333333703, 0.3079598441704289313, 0.3333333333333333703, 0.3079598441704289313, 0.3333333333333333703, 0.3079598441704289313, 0.3333333333333333703, 0.3079598441704289313, 0.3333333333333333703, 0.3079598441704289313, 0.3333333333333333703, 0.3079598441704289313, 0.3333333333333333703, 0.3079598441704289313, 0.3333333333333333703, 0.3079598441704289313, 0.3333333333333333703, 0.3079598441704289313, 0.3333333333333333703, 0.3079598441704289313, 0.3333333333333333703, 0.3079598441704289313, 0.3333333333333333703, 0.3079598441704289313, 0.3333333333333333703, 0.3079598441704289313, 0.3333333333333333703, 0.3079598441704289313, 0.3333333333333333703, 0.3079598441704289313, 0.3333333333333333703, 0.3079598441704289313, 0.3333333333333333703, 0.3079598441704289313, 0.3333333333333333703, 0.3079598441704289313, 0.3333333333333333703, 0.3079598441704289313, 0.3333333333333333703, 0.3079598441704289313, 0.3333333333333333703, 0.3079598441704289313, 0.3333333333333333703, 0.3079598441704289313, 0.3333333333333333703, 0.3079598441704289313, 0.3333333333333333703, 0.3079598441704289313, 0.3333333333333333703, 0.3079598441704289313, 0.3333333333333333703, 0.3079598441704289313, 0.3333333333333333703, 0.3079598441704289313, 0.3333333333333333703, 0.3079598441704289313, 0.3333333333333333703, 0.3079598441704289313, 0.3333333333333333703, 0.3079598441704289313, 0.3333333333333333703, 0.3079598441704289313, 0.3333333333333333703, 0.3079598441704289313, 0.3333333333333333703, 0.3079598441704289313, 0.3333333333333333703, 0.3079598441704289313, 0.3333333333333333703, 0.3079598441704289313, 0.3333333333333333703, 0.3079598441704289313, 0.3333333333333333703, 0.3079598441704289313, 0.3333333333333333703, 0.3079598441704289313, 0.3333333333333333703),
 ( 1.000000000000000000, 0.9238795325112867385, 1.000000000000000000, 0.9238795325112867385, 1.000000000000000000, 0.9238795325112867385, 1.000000000000000000, 0.9238795325112867385, 1.000000000000000000, 0.9238795325112867385, 1.000000000000000000, 0.9238795325112867385, 1.000000000000000000, 0.9238795325112867385, 1.000000000000000000, 0.9238795325112867385, 1.000000000000000000, 0.9238795325112867385, 1.000000000000000000, 0.9238795325112867385, 1.000000000000000000, 0.9238795325112867385, 1.000000000000000000, 0.9238795325112867385, 1.000000000000000000, 0.9238795325112867385, 1.000000000000000000, 0.9238795325112867385, 1.000000000000000000, 0.9238795325112867385, 1.000000000000000000, 0.9238795325112867385, 1.000000000000000000, 0.9238795325112867385, 1.000000000000000000, 0.9238795325112867385, 1.000000000000000000, 0.9238795325112867385, 1.000000000000000000, 0.9238795325112867385, 1.000000000000000000, 0.9238795325112867385, 1.000000000000000000, 0.9238795325112867385, 1.000000000000000000, 0.9238795325112867385, 1.000000000000000000, 0.9238795325112867385, 1.000000000000000000, 0.9238795325112867385, 1.000000000000000000, 0.9238795325112867385, 1.000000000000000000, 0.9238795325112867385, 1.000000000000000000, 0.9238795325112867385, 1.000000000000000000, 0.9238795325112867385, 1.000000000000000000, 0.9238795325112867385, 1.000000000000000000, 0.9238795325112867385, 1.000000000000000000, 0.9238795325112867385, 1.000000000000000000, 0.9238795325112867385, 1.000000000000000000, 0.9238795325112867385, 1.000000000000000000, 0.9238795325112867385, 1.000000000000000000, 0.9238795325112867385, 1.000000000000000000, 0.9238795325112867385, 1.000000000000000000, 0.9238795325112867385, 1.000000000000000000, 0.9238795325112867385, 1.000000000000000000, 0.9238795325112867385, 1.000000000000000000) ) ) 
 REPRESENTATION_ITEM ( '' )  SURFACE ( )  );
#2951 = CARTESIAN_POINT ( 'NONE',  ( -5.317658234375000070, -27.14843749948790119, 0.000000000000000000 ) ) ;
#2952 = DIRECTION ( 'NONE',  ( 0.000000000000000000, 1.000000000000000000, 0.000000000000000000 ) ) ;
#2953 = CARTESIAN_POINT ( 'NONE',  ( -1.406733260263395735, -27.35491455036742181, 5.250000000000000000 ) ) ;
#2954 = CARTESIAN_POINT ( 'NONE',  ( 0.01814118441321408565, -6.249340926099360871, -3.500000000000000000 ) ) ;
#2955 = CARTESIAN_POINT ( 'NONE',  ( -3.492485675378536047, -8.149340926099361226, -1.467888652719048670 ) ) ;
#2956 = ORIENTED_EDGE ( 'NONE', *, *, #2090, .T. ) ;
#2957 = CARTESIAN_POINT ( 'NONE',  ( 1.406733260263402174, -28.05133545031536357, 5.249999999999995559 ) ) ;
#2958 = CARTESIAN_POINT ( 'NONE',  ( 3.616337804771879580E-16, -28.54687500034139802, -5.905927827173866440 ) ) ;
#2959 = ORIENTED_EDGE ( 'NONE', *, *, #7430, .T. ) ;
#2960 = ORIENTED_EDGE ( 'NONE', *, *, #6666, .F. ) ;
#2961 = CARTESIAN_POINT ( 'NONE',  ( 1.406733260263385521, -29.67633545031537423, 5.250000000000006217 ) ) ;
#2962 = CARTESIAN_POINT ( 'NONE',  ( -2.692658234375000514, -27.40104166632526628, -4.663820869356205989 ) ) ;
#2963 = CARTESIAN_POINT ( 'NONE',  ( -4.000000000000000000, -0.2493409260993606769, -0.01814118441321865144 ) ) ;
#2964 = SURFACE_STYLE_FILL_AREA ( #3843 ) ;
#2965 = AXIS2_PLACEMENT_3D ( 'NONE', #8720, #2351, #5181 ) ;
#2966 = ORIENTED_EDGE ( 'NONE', *, *, #7789, .F. ) ;
#2967 = LINE ( 'NONE', #2355, #4889 ) ;
#2968 = CARTESIAN_POINT ( 'NONE',  ( -1.113604000661152470E-15, -29.59375000068279959, 6.062177826491070398 ) ) ;
#2969 = CARTESIAN_POINT ( 'NONE',  ( 5.250000000000000000, -29.78125000068279604, 0.000000000000000000 ) ) ;
#2970 = CARTESIAN_POINT ( 'NONE',  ( 3.616337804771879580E-16, -29.85937500034139802, -5.905927827173866440 ) ) ;
#2971 = CARTESIAN_POINT ( 'NONE',  ( -0.01814118441321365544, -2.249340926099361315, 3.500000000000000000 ) ) ;
#2972 = CARTESIAN_POINT ( 'NONE',  ( 0.000000000000000000, -9.999999999999998224, 0.000000000000000000 ) ) ;
#2973 = CARTESIAN_POINT ( 'NONE',  ( -1.224499502706077880, -1.549340926099361804, -3.007514324621463064 ) ) ;
#2974 = AXIS2_PLACEMENT_3D ( 'NONE', #8866, #9054, #2698 ) ;
#2975 = DIRECTION ( 'NONE',  ( 0.000000000000000000, -0.9973637043974449279, -0.07256473765270717025 ) ) ;
#2976 = CARTESIAN_POINT ( 'NONE',  ( -4.007514324621467949, -1.949340926099360827, 1.638713065079161924 ) ) ;
#2977 = CIRCLE ( 'NONE', #3717, 3.000000000000000444 ) ;
#2978 = CARTESIAN_POINT ( 'NONE',  ( 1.406733260263393293, -27.57366454968463643, -5.250000000000000000 ) ) ;
#2979 = CARTESIAN_POINT ( 'NONE',  ( -5.249999999999999112, -27.67708333401612464, -3.031088913245536975 ) ) ;
#2980 = AXIS2_PLACEMENT_3D ( 'NONE', #4346, #5174, #4534 ) ;
#2981 = CARTESIAN_POINT ( 'NONE',  ( -2.033577675846918216E-14, -29.12499999931720751, 5.250000000000000888 ) ) ;
#2982 = ORIENTED_EDGE ( 'NONE', *, *, #248, .T. ) ;
#2983 = DIRECTION ( 'NONE',  ( 1.000000000000000000, 0.000000000000000000, 0.000000000000000000 ) ) ;
#2984 = CARTESIAN_POINT ( 'NONE',  ( 2.692658234375002735, -28.74479166632526628, 4.663820869356205101 ) ) ;
#2985 = EDGE_CURVE ( 'NONE', #8235, #2142, #6371, .T. ) ;
#2986 = DIRECTION ( 'NONE',  ( -0.000000000000000000, -1.000000000000000000, -0.000000000000000000 ) ) ;
#2987 = ORIENTED_EDGE ( 'NONE', *, *, #4754, .T. ) ;
#2988 = CARTESIAN_POINT ( 'NONE',  ( 5.385316468749999252, -27.68229166632526272, -3.109213912904139399 ) ) ;
#2989 = CARTESIAN_POINT ( 'NONE',  ( 2.108492589042352705, -3.950659073900640195, -2.134148098076933397 ) ) ;
#2990 = PRESENTATION_LAYER_ASSIGNMENT (  '', '', ( #3292 ) ) ;
#2991 = ORIENTED_EDGE ( 'NONE', *, *, #5699, .F. ) ;
#2992 = CARTESIAN_POINT ( 'NONE',  ( 3.712013335537174572E-16, -28.93749999999999645, -6.062177826491070398 ) ) ;
#2993 = CARTESIAN_POINT ( 'NONE',  ( 5.249999999999997335, -29.77083333333332860, 3.031088913245538308 ) ) ;
#2994 = EDGE_CURVE ( 'NONE', #7024, #6114, #3567, .T. ) ;
#2995 = CARTESIAN_POINT ( 'NONE',  ( -5.114683531250000748, -27.54687500034139802, -6.263680815196995234E-16 ) ) ;
#2996 = AXIS2_PLACEMENT_3D ( 'NONE', #543, #1801, #6871 ) ;
#2997 = CARTESIAN_POINT ( 'NONE',  ( -5.114683531250000748, -27.52604166700806587, 2.952963913586931888 ) ) ;
#2998 = CARTESIAN_POINT ( 'NONE',  ( 3.673940397442060361E-16, 73.00000000000001421, 3.000000000000000444 ) ) ;
#2999 = CARTESIAN_POINT ( 'NONE',  ( 3.500000000000000000, -5.849340926099361404, 0.01814118441321387054 ) ) ;
#3000 = CARTESIAN_POINT ( 'NONE',  ( 1.185285273922203525E-14, -28.71875000068279959, -5.250000000000000000 ) ) ;
#3001 = DIRECTION ( 'NONE',  ( 0.000000000000000000, -0.000000000000000000, -1.000000000000000000 ) ) ;
#3002 = CARTESIAN_POINT ( 'NONE',  ( -5.250000000000000000, -29.65625000068279604, -6.429395695523604153E-16 ) ) ;
#3003 = CARTESIAN_POINT ( 'NONE',  ( 1.000000000000000000, -35.00000000000000000, -3.048902179152658931 ) ) ;
#3004 = EDGE_LOOP ( 'NONE', ( #2783, #9048 ) ) ;
#3005 = CARTESIAN_POINT ( 'NONE',  ( 1.406733260263395735, -27.17633545031536713, 5.250000000000000000 ) ) ;
#3006 = DIRECTION ( 'NONE',  ( 0.000000000000000000, 1.000000000000000000, 0.000000000000000000 ) ) ;
#3007 = CARTESIAN_POINT ( 'NONE',  ( -5.114683531250000748, -28.96354166700807298, 2.952963913586931888 ) ) ;
#3008 = ORIENTED_EDGE ( 'NONE', *, *, #3394, .T. ) ;
#3009 = FACE_OUTER_BOUND ( 'NONE', #6960, .T. ) ;
#3010 = CARTESIAN_POINT ( 'NONE',  ( 5.385316468750001029, -27.25520833299193413, 3.109213912904134958 ) ) ;
#3011 = CARTESIAN_POINT ( 'NONE',  ( -0.01814118441313417734, -7.350659073900637885, -4.000000000000000000 ) ) ;
#3012 = CARTESIAN_POINT ( 'NONE',  ( 0.000000000000000000, -29.87813065659485190, 0.000000000000000000 ) ) ;
#3013 = VERTEX_POINT ( 'NONE', #4897 ) ;
#3014 = CARTESIAN_POINT ( 'NONE',  ( -1.000000000000000000, -20.00000000000000000, -1.118033988749894680 ) ) ;
#3015 = EDGE_CURVE ( 'NONE', #8099, #6175, #4626, .T. ) ;
#3016 = CARTESIAN_POINT ( 'NONE',  ( 5.385316468750000141, -27.98437499965860198, -6.595110575850215044E-16 ) ) ;
#3017 = PRODUCT_DEFINITION_CONTEXT ( 'detailed design', #5270, 'design' ) ;
#3018 = CARTESIAN_POINT ( 'NONE',  ( 5.114683531249998971, -27.38020833367473017, 2.952963913586936329 ) ) ;
#3019 = LINE ( 'NONE', #3069, #197 ) ;
#3020 = CARTESIAN_POINT ( 'NONE',  ( -2.692658234374996518, -27.28645833299193413, 4.663820869356208654 ) ) ;
#3021 = CARTESIAN_POINT ( 'NONE',  ( 2.134148098076933397, -1.950659073900639306, 2.108492589042352261 ) ) ;
#3022 = UNCERTAINTY_MEASURE_WITH_UNIT (LENGTH_MEASURE( 1.000000000000000082E-05 ), #2152, 'distance_accuracy_value', 'NONE');
#3023 = FACE_OUTER_BOUND ( 'NONE', #2465, .T. ) ;
#3024 = CARTESIAN_POINT ( 'NONE',  ( -4.000000000000000000, -0.2493409260993606769, -0.01814118441321865144 ) ) ;
#3025 = AXIS2_PLACEMENT_3D ( 'NONE', #3354, #599, #1958 ) ;
#3026 = COLOUR_RGB ( '',0.8941176470588234615, 0.8941176470588234615, 0.8941176470588234615 ) ;
#3027 = CARTESIAN_POINT ( 'NONE',  ( 2.624999999999998668, -28.27083333265053255, -4.546633369868303021 ) ) ;
#3028 = DIRECTION ( 'NONE',  ( 0.000000000000000000, 1.000000000000000000, 0.000000000000000000 ) ) ;
#3029 = CARTESIAN_POINT ( 'NONE',  ( -3.500000000000000000, -3.449340926099361049, -0.01814118441321344033 ) ) ;
#3030 = CARTESIAN_POINT ( 'NONE',  ( 1.975475456537005874E-15, -29.62499999931719685, 5.250000000000000000 ) ) ;
#3031 = ORIENTED_EDGE ( 'NONE', *, *, #8536, .F. ) ;
#3032 = CIRCLE ( 'NONE', #7773, 2.999999999999999556 ) ;
#3033 =( BOUNDED_CURVE ( )  B_SPLINE_CURVE ( 2, ( #1588, #3089, #8754, #5065, #891, #6562, #2385, #1494, #7919, #193, #8251, #379, #8294, #3322, #6102, #6005, #4571, #8156, #8932, #330, #3880, #1784, #8799, #3228, #4018, #3828, #8887, #1175, #1884, #3141, #7457, #476, #3272, #4755, #6654, #2581, #6049, #2528, #8844, #5353, #4664, #2481, #8981, #4618, #8202, #2630, #5401, #6702, #425, #6800, #1083, #284, #5449, #3925, #6853, #3971, #4709, #7548, #6153, #1131, #1832, #3184, #1927, #2435, #981, #8106, #5961, #5261, #1734, #5304, #7407, #1030, #6753, #7503, #8519, #7030, #7732, #3454, #3499, #695, #4063, #568, #1223, #7641, #7777, #6939, #8344, #657, #5584, #3367, #3540, #2014, #6322, #9158, #2807, #6283, #7599, #1969, #7684, #2855, #5671, #3412, #5542, #4150, #4798, #1356, #8387, #6902, #6241, #5497, #2717, #5627, #8476, #1308, #6365, #1269, #2101, #526, #9075, #2146, #6985, #4, #4839, #6198, #4924, #4107, #1399, #8428, #4240, #613, #2056, #7071, #4881, #9119, #9026, #2672, #2764, #4195, #1437, #1581, #4329, #3730, #2897, #1629, #2329 ),
 .UNSPECIFIED., .F., .T. ) 
 B_SPLINE_CURVE_WITH_KNOTS ( ( 3, 2, 2, 2, 2, 2, 2, 2, 2, 2, 2, 2, 2, 2, 2, 2, 2, 2, 2, 2, 2, 2, 2, 2, 2, 2, 2, 2, 2, 2, 2, 2, 2, 2, 2, 2, 2, 2, 2, 2, 2, 2, 2, 2, 2, 2, 2, 2, 2, 2, 2, 2, 2, 2, 2, 2, 2, 2, 2, 2, 2, 2, 2, 2, 2, 2, 2, 2, 2, 2, 2, 2, 3 ),
 ( 0.000000000000000000, 0.01388888888888888812, 0.02777777777777777624, 0.04166666666666666435, 0.05555555555555555247, 0.06944444444444444753, 0.08333333333333332871, 0.09722222222222222376, 0.1111111111111111049, 0.1250000000000000000, 0.1388888888888888951, 0.1527777777777777901, 0.1666666666666666574, 0.1805555555555555525, 0.1944444444444444475, 0.2083333333333333426, 0.2222222222222222099, 0.2361111111111111049, 0.2500000000000000000, 0.2638888888888888951, 0.2777777777777777901, 0.2916666666666666852, 0.3055555555555555802, 0.3194444444444444198, 0.3333333333333333148, 0.3472222222222222099, 0.3611111111111111049, 0.3750000000000000000, 0.3888888888888888951, 0.4027777777777777901, 0.4166666666666666852, 0.4305555555555555802, 0.4444444444444444198, 0.4583333333333333148, 0.4722222222222222099, 0.4861111111111111049, 0.5000000000000000000, 0.5138888888888888395, 0.5277777777777777901, 0.5416666666666666297, 0.5555555555555555802, 0.5694444444444444198, 0.5833333333333333703, 0.5972222222222222099, 0.6111111111111111605, 0.6250000000000000000, 0.6388888888888888395, 0.6527777777777777901, 0.6666666666666666297, 0.6805555555555555802, 0.6944444444444444198, 0.7083333333333333703, 0.7222222222222222099, 0.7361111111111111605, 0.7500000000000000000, 0.7638888888888888395, 0.7777777777777777901, 0.7916666666666666297, 0.8055555555555555802, 0.8194444444444444198, 0.8333333333333333703, 0.8472222222222222099, 0.8611111111111111605, 0.8750000000000000000, 0.8888888888888888395, 0.9027777777777777901, 0.9166666666666666297, 0.9305555555555555802, 0.9444444444444444198, 0.9583333333333333703, 0.9722222222222222099, 0.9861111111111111605, 1.000000000000000000 ),
 .UNSPECIFIED. ) 
 CURVE ( )  GEOMETRIC_REPRESENTATION_ITEM ( )  RATIONAL_B_SPLINE_CURVE ( ( 1.000000000000000000, 0.8660254037844387076, 1.000000000000000000, 0.8660254037844387076, 1.000000000000000000, 0.8660254037844387076, 1.000000000000000000, 0.8660254037844387076, 1.000000000000000000, 0.8660254037844387076, 1.000000000000000000, 0.8660254037844387076, 1.000000000000000000, 0.8660254037844387076, 1.000000000000000000, 0.8660254037844387076, 1.000000000000000000, 0.8660254037844387076, 1.000000000000000000, 0.8660254037844387076, 1.000000000000000000, 0.8660254037844387076, 1.000000000000000000, 0.8660254037844387076, 1.000000000000000000, 0.8660254037844387076, 1.000000000000000000, 0.8660254037844387076, 1.000000000000000000, 0.8660254037844387076, 1.000000000000000000, 0.8660254037844387076, 1.000000000000000000, 0.8660254037844387076, 1.000000000000000000, 0.8660254037844387076, 1.000000000000000000, 0.8660254037844387076, 1.000000000000000000, 0.8660254037844387076, 1.000000000000000000, 0.8660254037844387076, 1.000000000000000000, 0.8660254037844387076, 1.000000000000000000, 0.8660254037844387076, 1.000000000000000000, 0.8660254037844387076, 1.000000000000000000, 0.8660254037844387076, 1.000000000000000000, 0.8660254037844387076, 1.000000000000000000, 0.8660254037844387076, 1.000000000000000000, 0.8660254037844387076, 1.000000000000000000, 0.8660254037844387076, 1.000000000000000000, 0.8660254037844387076, 1.000000000000000000, 0.8660254037844387076, 1.000000000000000000, 0.8660254037844387076, 1.000000000000000000, 0.8660254037844387076, 1.000000000000000000, 0.8660254037844387076, 1.000000000000000000, 0.8660254037844387076, 1.000000000000000000, 0.8660254037844387076, 1.000000000000000000, 0.8660254037844387076, 1.000000000000000000, 0.8660254037844387076, 1.000000000000000000, 0.8660254037844387076, 1.000000000000000000, 0.8660254037844387076, 1.000000000000000000, 0.8660254037844387076, 1.000000000000000000, 0.8660254037844387076, 1.000000000000000000, 0.8660254037844387076, 1.000000000000000000, 0.8660254037844387076, 1.000000000000000000, 0.8660254037844387076, 1.000000000000000000, 0.8660254037844387076, 1.000000000000000000, 0.8660254037844387076, 1.000000000000000000, 0.8660254037844387076, 1.000000000000000000, 0.8660254037844387076, 1.000000000000000000, 0.8660254037844387076, 1.000000000000000000, 0.8660254037844387076, 1.000000000000000000, 0.8660254037844387076, 1.000000000000000000, 0.8660254037844387076, 1.000000000000000000, 0.8660254037844387076, 1.000000000000000000, 0.8660254037844387076, 1.000000000000000000, 0.8660254037844387076, 1.000000000000000000, 0.8660254037844387076, 1.000000000000000000, 0.8660254037844387076, 1.000000000000000000, 0.8660254037844387076, 1.000000000000000000, 0.8660254037844387076, 1.000000000000000000, 0.8660254037844387076, 1.000000000000000000, 0.8660254037844387076, 1.000000000000000000, 0.8660254037844387076, 1.000000000000000000, 0.8660254037844387076, 1.000000000000000000, 0.8660254037844387076, 1.000000000000000000, 0.8660254037844387076, 1.000000000000000000, 0.8660254037844387076, 1.000000000000000000, 0.8660254037844387076, 1.000000000000000000, 0.8660254037844387076, 1.000000000000000000, 0.8660254037844387076, 1.000000000000000000, 0.8660254037844387076, 1.000000000000000000, 0.8660254037844387076, 1.000000000000000000 ) ) 
 REPRESENTATION_ITEM ( '' )  );
#3034 = CARTESIAN_POINT ( 'NONE',  ( 2.692658234375002735, -27.74479166632526628, 4.663820869356205101 ) ) ;
#3035 = CARTESIAN_POINT ( 'NONE',  ( 0.01814118441321938349, -6.249340926099361759, -4.000000000000000000 ) ) ;
#3036 = VECTOR ( 'NONE', #7187, 1000.000000000000000 ) ;
#3037 = CARTESIAN_POINT ( 'NONE',  ( -1.406733260263397289, -28.44866454968463998, 5.249999999999997335 ) ) ;
#3038 = ORIENTED_EDGE ( 'NONE', *, *, #1575, .F. ) ;
#3039 = DIRECTION ( 'NONE',  ( -0.000000000000000000, -1.000000000000000000, -0.000000000000000000 ) ) ;
#3040 = CARTESIAN_POINT ( 'NONE',  ( 1.260781871532430598, -6.650659073900641260, 2.992485675378564469 ) ) ;
#3041 = ORIENTED_EDGE ( 'NONE', *, *, #1120, .F. ) ;
#3042 = CARTESIAN_POINT ( 'NONE',  ( -5.250000000000000000, -28.12499999999999645, -6.429395695523604153E-16 ) ) ;
#3043 = CIRCLE ( 'NONE', #8238, 4.000000000000000000 ) ;
#3044 = CARTESIAN_POINT ( 'NONE',  ( 2.557341765624996821, -28.21354166700806587, 4.429445870380401828 ) ) ;
#3045 = FILL_AREA_STYLE_COLOUR ( '', #6641 ) ;
#3046 = CARTESIAN_POINT ( 'NONE',  ( -2.625000000000002220, -29.36458333401613174, 4.546633369868302132 ) ) ;
#3047 = CARTESIAN_POINT ( 'NONE',  ( 0.000000000000000000, 73.00000000000001421, 0.000000000000000000 ) ) ;
#3048 = CARTESIAN_POINT ( 'NONE',  ( -3.507514324621464397, -3.549340926099361582, 1.431606283892619347 ) ) ;
#3049 = EDGE_CURVE ( 'NONE', #3470, #8050, #6836, .T. ) ;
#3050 = CARTESIAN_POINT ( 'NONE',  ( -2.624999999999996891, -29.89583333265053611, 4.546633369868304797 ) ) ;
#3051 = DIRECTION ( 'NONE',  ( -0.000000000000000000, 1.000000000000000000, -0.000000000000000000 ) ) ;
#3052 = CARTESIAN_POINT ( 'NONE',  ( -2.462045979635576920, -6.449340926099361937, -2.487701488670255756 ) ) ;
#3053 = ORIENTED_EDGE ( 'NONE', *, *, #3787, .T. ) ;
#3054 = CARTESIAN_POINT ( 'NONE',  ( 1.406733260263398400, -28.01116454900182973, -5.249999999999997335 ) ) ;
#3055 = PLANE ( 'NONE',  #147 ) ;
#3056 = CARTESIAN_POINT ( 'NONE',  ( -2.557341765624999042, -28.02604166700806587, -4.429445870380400052 ) ) ;
#3057 = VERTEX_POINT ( 'NONE', #2031 ) ;
#3058 = CARTESIAN_POINT ( 'NONE',  ( -2.033577675846918216E-14, -29.68750000000000355, 5.250000000000000888 ) ) ;
#3059 = EDGE_CURVE ( 'NONE', #2122, #4547, #4854, .T. ) ;
#3060 = CARTESIAN_POINT ( 'NONE',  ( 2.692658234374998738, -27.94270833299193413, -4.663820869356206877 ) ) ;
#3061 = CARTESIAN_POINT ( 'NONE',  ( -0.01814118441313417734, -4.150659073900638596, -4.000000000000000000 ) ) ;
#3062 = CARTESIAN_POINT ( 'NONE',  ( 5.249999999999997335, -27.52083333333332860, 3.031088913245538308 ) ) ;
#3063 = ORIENTED_EDGE ( 'NONE', *, *, #905, .F. ) ;
#3064 = EDGE_CURVE ( 'NONE', #8472, #7496, #890, .T. ) ;
#3065 = FACE_OUTER_BOUND ( 'NONE', #1876, .T. ) ;
#3066 = CARTESIAN_POINT ( 'NONE',  ( 2.625000000000000444, -28.98958333401613174, -4.546633369868303021 ) ) ;
#3067 = CARTESIAN_POINT ( 'NONE',  ( 2.692658234374998738, -27.94270833299193413, -4.663820869356206877 ) ) ;
#3068 = CARTESIAN_POINT ( 'NONE',  ( -5.114683531250000748, -27.71354166700806587, 2.952963913586931888 ) ) ;
#3069 = CARTESIAN_POINT ( 'NONE',  ( 6.429395695523604153E-16, -30.00000000000000000, -5.250000000000000000 ) ) ;
#3070 = DIRECTION ( 'NONE',  ( 0.000000000000000000, 1.000000000000000000, 0.000000000000000000 ) ) ;
#3071 = CARTESIAN_POINT ( 'NONE',  ( -1.260781871532431708, -1.050659073900639617, -2.992485675378564469 ) ) ;
#3072 = CARTESIAN_POINT ( 'NONE',  ( -1.638713065079163034, -1.549340926099360916, -4.007514324621466173 ) ) ;
#3073 = CARTESIAN_POINT ( 'NONE',  ( -2.625000000000000444, -27.72916666598386826, -4.546633369868303021 ) ) ;
#3074 = CARTESIAN_POINT ( 'NONE',  ( 5.250000000000000000, -27.62500000000000000, -6.429395695523604153E-16 ) ) ;
#3075 = CARTESIAN_POINT ( 'NONE',  ( -1.431606283892620235, -3.149340926099361671, -3.507514324621463953 ) ) ;
#3076 = PLANE ( 'NONE',  #8474 ) ;
#3077 = FILL_AREA_STYLE ('',( #8043 ) ) ;
#3078 = CARTESIAN_POINT ( 'NONE',  ( 5.385316468749999252, -28.68229166632526983, -3.109213912904139399 ) ) ;
#3079 = CARTESIAN_POINT ( 'NONE',  ( 4.000000000000000000, -4.249340926099360871, 0.01814118441321914063 ) ) ;
#3080 = CARTESIAN_POINT ( 'NONE',  ( 2.300847884672513123E-14, -27.43750000000000355, -5.250000000000000000 ) ) ;
#3081 = VERTEX_POINT ( 'NONE', #107 ) ;
#3082 = CARTESIAN_POINT ( 'NONE',  ( -5.249999999999997335, -27.22916666666666430, 3.031088913245538308 ) ) ;
#3083 = CARTESIAN_POINT ( 'NONE',  ( 2.108492589042352705, -7.150659073900638596, -2.134148098076933397 ) ) ;
#3084 = EDGE_LOOP ( 'NONE', ( #7913, #1646 ) ) ;
#3085 = CARTESIAN_POINT ( 'NONE',  ( -5.250000000000000000, -27.89583333333332860, -3.031088913245536531 ) ) ;
#3086 = CARTESIAN_POINT ( 'NONE',  ( 3.616337804771879580E-16, -27.85937500034139802, -5.905927827173866440 ) ) ;
#3087 =( BOUNDED_CURVE ( )  B_SPLINE_CURVE ( 2, ( #6880, #1955, #2171, #6308, #4265, #1515, #31, #3571, #2881 ),
 .UNSPECIFIED., .F., .T. ) 
 B_SPLINE_CURVE_WITH_KNOTS ( ( 3, 2, 2, 2, 3 ),
 ( 0.6041666666666667407, 0.6111111111111111605, 0.6250000000000000000, 0.6388888888888888395, 0.6458333333333333703 ),
 .UNSPECIFIED. ) 
 CURVE ( )  GEOMETRIC_REPRESENTATION_ITEM ( )  RATIONAL_B_SPLINE_CURVE ( ( 0.9330127018922192983, 0.9330127018922198534, 1.000000000000000000, 0.8660254037844387076, 1.000000000000000000, 0.8660254037844387076, 1.000000000000000000, 0.9330127018922187432, 0.9330127018922192983 ) ) 
 REPRESENTATION_ITEM ( '' )  );
#3088 = CARTESIAN_POINT ( 'NONE',  ( -5.250000000000000000, -27.50000000000000000, 0.000000000000000000 ) ) ;
#3089 = CARTESIAN_POINT ( 'NONE',  ( 5.114683531250000748, -29.83854166700806232, -2.952963913586932776 ) ) ;
#3090 = CARTESIAN_POINT ( 'NONE',  ( 0.01814118441321408565, -3.049340926099361138, -3.500000000000000000 ) ) ;
#3091 = CARTESIAN_POINT ( 'NONE',  ( 2.161402558328724325E-14, -28.56250000000000000, -5.250000000000000000 ) ) ;
#3092 = FACE_OUTER_BOUND ( 'NONE', #1506, .T. ) ;
#3093 = CARTESIAN_POINT ( 'NONE',  ( -1.084901341431563923E-15, -28.23437500034139802, 5.905927827173866440 ) ) ;
#3094 = COLOUR_RGB ( '',0.8941176470588234615, 0.8941176470588234615, 0.8941176470588234615 ) ;
#3095 = CARTESIAN_POINT ( 'NONE',  ( 0.000000000000000000, 1.000000000000000888, 0.000000000000000000 ) ) ;
#3096 = ORIENTED_EDGE ( 'NONE', *, *, #4416, .F. ) ;
#3097 = CARTESIAN_POINT ( 'NONE',  ( -5.250000000000000000, -29.37500000000000000, -6.429395695523604153E-16 ) ) ;
#3098 = CARTESIAN_POINT ( 'NONE',  ( 3.616337804771879580E-16, -28.79687500034139802, -5.905927827173866440 ) ) ;
#3099 = ORIENTED_EDGE ( 'NONE', *, *, #9098, .T. ) ;
#3100 = DIRECTION ( 'NONE',  ( 0.000000000000000000, 1.000000000000000000, 0.000000000000000000 ) ) ;
#3101 = LINE ( 'NONE', #3841, #41 ) ;
#3102 = CARTESIAN_POINT ( 'NONE',  ( 1.674995433905515085, -5.050659073900638951, 3.992485675378568022 ) ) ;
#3103 = EDGE_CURVE ( 'NONE', #1439, #3872, #8432, .T. ) ;
#3104 = CARTESIAN_POINT ( 'NONE',  ( 2.692658234375002735, -27.77604166632526628, 4.663820869356205101 ) ) ;
#3105 = VERTEX_POINT ( 'NONE', #7320 ) ;
#3106 = EDGE_CURVE ( 'NONE', #1171, #8145, #5500, .T. ) ;
#3107 = CARTESIAN_POINT ( 'NONE',  ( -5.249999999999997335, -27.91666666598387181, 3.031088913245538308 ) ) ;
#3108 = CARTESIAN_POINT ( 'NONE',  ( 5.250000000000000000, -29.28125000068279604, 0.000000000000000000 ) ) ;
#3109 = CARTESIAN_POINT ( 'NONE',  ( 5.385316468750000141, -27.73437499965860198, -6.595110575850215044E-16 ) ) ;
#3110 = CARTESIAN_POINT ( 'NONE',  ( 5.114683531250000748, -27.60937500034139802, 0.000000000000000000 ) ) ;
#3111 = VERTEX_POINT ( 'NONE', #4436 ) ;
#3112 = AXIS2_PLACEMENT_3D ( 'NONE', #823, #5047, #7062 ) ;
#3113 = CARTESIAN_POINT ( 'NONE',  ( 2.625000000000002220, -28.85416666598386826, 4.546633369868302132 ) ) ;
#3114 = ADVANCED_FACE ( 'NONE', ( #7272 ), #2300, .T. ) ;
#3115 = CARTESIAN_POINT ( 'NONE',  ( 3.007514324621436863, -5.250659073900640017, 1.224499502706140719 ) ) ;
#3116 = CARTESIAN_POINT ( 'NONE',  ( 5.182341765625000818, -26.82031250051209526, 0.000000000000000000 ) ) ;
#3117 = CARTESIAN_POINT ( 'NONE',  ( 5.250000000000000000, -27.54166666598386470, -3.031088913245536531 ) ) ;
#3118 = CARTESIAN_POINT ( 'NONE',  ( -3.250000000000000444, 0.000000000000000000, -3.404030812060692501E-14 ) ) ;
#3119 = CIRCLE ( 'NONE', #4298, 3.500000000000000444 ) ;
#3120 = CARTESIAN_POINT ( 'NONE',  ( 1.467888652719048226, -4.549340926099360694, -3.492485675378535603 ) ) ;
#3121 = PLANE ( 'NONE',  #1635 ) ;
#3122 = CARTESIAN_POINT ( 'NONE',  ( 1.406733260263405061, -27.69866454968462932, -5.249999999999994671 ) ) ;
#3123 = DIRECTION ( 'NONE',  ( 1.000000000000000000, 0.000000000000000000, 0.000000000000000000 ) ) ;
#3124 = CARTESIAN_POINT ( 'NONE',  ( -5.385316468749998364, -28.55729166632527338, 3.109213912904140287 ) ) ;
#3125 = CARTESIAN_POINT ( 'NONE',  ( 1.638713065079161924, -7.149340926099361226, 4.007514324621467949 ) ) ;
#3126 = CARTESIAN_POINT ( 'NONE',  ( -2.624999999999998668, -27.41666666666666430, -4.546633369868303021 ) ) ;
#3127 = EDGE_LOOP ( 'NONE', ( #3914, #7118 ) ) ;
#3128 = AXIS2_PLACEMENT_3D ( 'NONE', #2198, #5020, #1497 ) ;
#3129 = CARTESIAN_POINT ( 'NONE',  ( 2.692658234375002735, -28.24479166632526628, 4.663820869356205101 ) ) ;
#3130 = CARTESIAN_POINT ( 'NONE',  ( 2.108492589042352705, -5.550659073900639839, -2.134148098076933397 ) ) ;
#3131 = EDGE_LOOP ( 'NONE', ( #8535, #369 ) ) ;
#3132 = CARTESIAN_POINT ( 'NONE',  ( -5.250000000000000888, -28.10416666666666430, 3.031088913245532979 ) ) ;
#3133 = AXIS2_PLACEMENT_3D ( 'NONE', #3047, #3741, #8659 ) ;
#3134 = EDGE_CURVE ( 'NONE', #6430, #7910, #1720, .T. ) ;
#3135 = EDGE_CURVE ( 'NONE', #6474, #1822, #5027, .T. ) ;
#3136 = ORIENTED_EDGE ( 'NONE', *, *, #2325, .T. ) ;
#3137 = PRESENTATION_STYLE_ASSIGNMENT (( #7260 ) ) ;
#3138 = CARTESIAN_POINT ( 'NONE',  ( -3.712013335537174572E-16, -27.56250000000000000, -6.062177826491070398 ) ) ;
#3139 = AXIS2_PLACEMENT_3D ( 'NONE', #2790, #7100, #4360 ) ;
#3140 = ORIENTED_EDGE ( 'NONE', *, *, #7764, .F. ) ;
#3141 = CARTESIAN_POINT ( 'NONE',  ( -5.114683531250000748, -29.25520833367473017, -2.952963913586935440 ) ) ;
#3142 = CARTESIAN_POINT ( 'NONE',  ( 3.507514324621465285, -1.149340926099361226, -1.431606283892619125 ) ) ;
#3143 = FACE_OUTER_BOUND ( 'NONE', #5079, .T. ) ;
#3144 = CARTESIAN_POINT ( 'NONE',  ( -5.250000000000000000, -30.09374999965860198, 0.000000000000000000 ) ) ;
#3145 = CARTESIAN_POINT ( 'NONE',  ( -5.114683531250000748, -28.77604166700806587, 2.952963913586931888 ) ) ;
#3146 = ORIENTED_EDGE ( 'NONE', *, *, #5233, .T. ) ;
#3147 = CARTESIAN_POINT ( 'NONE',  ( 1.975475456537005874E-15, -27.68749999999999289, 5.249999999999999112 ) ) ;
#3148 = VECTOR ( 'NONE', #1921, 1000.000000000000000 ) ;
#3149 = CARTESIAN_POINT ( 'NONE',  ( 0.000000000000000000, 69.99999999999998579, 0.000000000000000000 ) ) ;
#3150 = ORIENTED_EDGE ( 'NONE', *, *, #4703, .F. ) ;
#3151 = CARTESIAN_POINT ( 'NONE',  ( 0.000000000000000000, -30.00000000000000000, 0.000000000000000000 ) ) ;
#3152 = CARTESIAN_POINT ( 'NONE',  ( -5.385316468750000141, -28.10937499965860198, 0.000000000000000000 ) ) ;
#3153 = CARTESIAN_POINT ( 'NONE',  ( 2.841254879263473310, -3.550659073900638063, 2.815599370228907272 ) ) ;
#3154 = CARTESIAN_POINT ( 'NONE',  ( 5.385316468750001029, -27.50520833299193768, 3.109213912904135846 ) ) ;
#3155 = ORIENTED_EDGE ( 'NONE', *, *, #1671, .F. ) ;
#3156 = CARTESIAN_POINT ( 'NONE',  ( 5.250000000000000000, -29.87500000000000000, -6.429395695523604153E-16 ) ) ;
#3157 = CARTESIAN_POINT ( 'NONE',  ( -5.250000000000000888, -29.38541666734946389, 3.031088913245532979 ) ) ;
#3158 = CARTESIAN_POINT ( 'NONE',  ( -3.807688866302469071E-16, -28.42187499965859843, -6.218427825808274356 ) ) ;
#3159 = ORIENTED_EDGE ( 'NONE', *, *, #5756, .F. ) ;
#3160 = FACE_OUTER_BOUND ( 'NONE', #9177, .T. ) ;
#3161 = CARTESIAN_POINT ( 'NONE',  ( 0.01814118441314514080, -3.350659073900639662, 3.000000000000000444 ) ) ;
#3162 = CARTESIAN_POINT ( 'NONE',  ( 0.000000000000000000, 69.99999999999998579, 5.250000000000000000 ) ) ;
#3163 = ADVANCED_FACE ( 'NONE', ( #989, #5222 ), #3055, .T. ) ;
#3164 = CARTESIAN_POINT ( 'NONE',  ( 5.250000000000000000, -28.04166666598386826, -3.031088913245536531 ) ) ;
#3165 = LINE ( 'NONE', #7990, #1845 ) ;
#3166 = CARTESIAN_POINT ( 'NONE',  ( 1.431606283892619347, -3.949340926099361049, 3.507514324621464397 ) ) ;
#3167 = CARTESIAN_POINT ( 'NONE',  ( 0.000000000000000000, 74.00000000000001421, 0.000000000000000000 ) ) ;
#3168 = DIRECTION ( 'NONE',  ( 0.000000000000000000, 0.000000000000000000, -1.000000000000000000 ) ) ;
#3169 = DIRECTION ( 'NONE',  ( 1.000000000000000000, 0.000000000000000000, 0.000000000000000000 ) ) ;
#3170 = CARTESIAN_POINT ( 'NONE',  ( 5.385316468749999252, -28.18229166632526628, -3.109213912904139399 ) ) ;
#3171 = CARTESIAN_POINT ( 'NONE',  ( 2.841254879263533262, -2.849340926099360960, -2.815599370228847320 ) ) ;
#3172 = VERTEX_POINT ( 'NONE', #6618 ) ;
#3173 = CARTESIAN_POINT ( 'NONE',  ( -2.692658234375000514, -28.11979166632526628, -4.663820869356205989 ) ) ;
#3174 = EDGE_CURVE ( 'NONE', #7207, #5259, #6830, .T. ) ;
#3175 = CARTESIAN_POINT ( 'NONE',  ( 3.500000000000000000, -5.350659073900638774, -0.01814118441313969030 ) ) ;
#3176 = AXIS2_PLACEMENT_3D ( 'NONE', #833, #4967, #2186 ) ;
#3177 = EDGE_LOOP ( 'NONE', ( #3063, #8649, #3733, #1324 ) ) ;
#3178 = CARTESIAN_POINT ( 'NONE',  ( 5.249999999999999112, -27.52083333333332860, 3.031088913245538308 ) ) ;
#3179 = CARTESIAN_POINT ( 'NONE',  ( -2.557341765625002594, -27.00520833367473017, 4.429445870380399164 ) ) ;
#3180 = CIRCLE ( 'NONE', #4212, 3.000000000000000444 ) ;
#3181 = ORIENTED_EDGE ( 'NONE', *, *, #3839, .F. ) ;
#3182 = CARTESIAN_POINT ( 'NONE',  ( 2.625000000000002220, -27.16666666666666430, 4.546633369868302132 ) ) ;
#3183 = ORIENTED_EDGE ( 'NONE', *, *, #8443, .F. ) ;
#3184 = CARTESIAN_POINT ( 'NONE',  ( 5.114683531250000748, -28.58854166700806587, -2.952963913586932776 ) ) ;
#3185 = CARTESIAN_POINT ( 'NONE',  ( 2.462045979635577364, -5.649340926099361226, 2.487701488670255312 ) ) ;
#3186 = DIRECTION ( 'NONE',  ( 0.000000000000000000, 0.9973637043974448169, 0.07256473765270714249 ) ) ;
#3187 = FACE_OUTER_BOUND ( 'NONE', #1122, .T. ) ;
#3188 = CARTESIAN_POINT ( 'NONE',  ( -2.557341765624999042, -28.33854166700806587, -4.429445870380400052 ) ) ;
#3189 = CARTESIAN_POINT ( 'NONE',  ( 5.250000000000000000, -27.28125000068279604, 0.000000000000000000 ) ) ;
#3190 = AXIS2_PLACEMENT_3D ( 'NONE', #4927, #616, #745 ) ;
#3191 = DIRECTION ( 'NONE',  ( 0.000000000000000000, -1.000000000000000000, 0.000000000000000000 ) ) ;
#3192 = CARTESIAN_POINT ( 'NONE',  ( 2.557341765625000818, -29.88020833367473372, -4.429445870380400052 ) ) ;
#3193 = EDGE_LOOP ( 'NONE', ( #9157, #7006 ) ) ;
#3194 = CARTESIAN_POINT ( 'NONE',  ( 5.250000000000000888, -27.89583333333332860, 3.031088913245533423 ) ) ;
#3195 = CARTESIAN_POINT ( 'NONE',  ( -5.385316468749998364, -29.33854166632526983, 3.109213912904140287 ) ) ;
#3196 = CARTESIAN_POINT ( 'NONE',  ( 1.674995433905601239, -1.349340926099360960, -3.992485675378532939 ) ) ;
#3197 = CARTESIAN_POINT ( 'NONE',  ( 5.250000000000000000, -30.00000000000000000, 0.000000000000000000 ) ) ;
#3198 = CARTESIAN_POINT ( 'NONE',  ( 2.692658234374998738, -29.19270833299193413, -4.663820869356206877 ) ) ;
#3199 = VERTEX_POINT ( 'NONE', #8713 ) ;
#3200 = SHAPE_REPRESENTATION ( 'barrel', ( #888 ), #7729 ) ;
#3201 = CARTESIAN_POINT ( 'NONE',  ( 3.712013335537174572E-16, -27.71875000068279249, -6.062177826491070398 ) ) ;
#3202 = EDGE_CURVE ( 'NONE', #3429, #7256, #6382, .T. ) ;
#3203 = CARTESIAN_POINT ( 'NONE',  ( 2.692658234375002735, -27.27604166632526628, 4.663820869356205101 ) ) ;
#3204 = PRODUCT_DEFINITION_CONTEXT ( 'detailed design', #5531, 'design' ) ;
#3205 = VERTEX_POINT ( 'NONE', #2392 ) ;
#3206 = CARTESIAN_POINT ( 'NONE',  ( 2.692658234375002735, -28.74479166632526628, 4.663820869356205101 ) ) ;
#3207 = CARTESIAN_POINT ( 'NONE',  ( -2.992485675378564469, 0.1493409260993606713, 1.260781871532430820 ) ) ;
#3208 = DIRECTION ( 'NONE',  ( 0.000000000000000000, 1.000000000000000000, 0.000000000000000000 ) ) ;
#3209 = FILL_AREA_STYLE ('',( #1997 ) ) ;
#3210 = DIRECTION ( 'NONE',  ( 0.000000000000000000, 1.000000000000000000, 0.000000000000000000 ) ) ;
#3211 = CARTESIAN_POINT ( 'NONE',  ( -2.487701488670255312, -0.4493409260993610488, 2.462045979635577808 ) ) ;
#3212 = CARTESIAN_POINT ( 'NONE',  ( -2.557341765625002594, -29.44270833367473017, 4.429445870380399164 ) ) ;
#3213 = ORIENTED_EDGE ( 'NONE', *, *, #8410, .F. ) ;
#3214 = CARTESIAN_POINT ( 'NONE',  ( -2.692658234374996518, -29.28645833299193413, 4.663820869356208654 ) ) ;
#3215 = CARTESIAN_POINT ( 'NONE',  ( -4.000000000000000000, -3.449340926099361049, -0.01814118441321865144 ) ) ;
#3216 = CARTESIAN_POINT ( 'NONE',  ( 0.000000000000000000, -27.00000000000000000, 0.000000000000000000 ) ) ;
#3217 = ORIENTED_EDGE ( 'NONE', *, *, #5142, .F. ) ;
#3218 = CARTESIAN_POINT ( 'NONE',  ( -2.692658234375000514, -28.36979166632526628, -4.663820869356205989 ) ) ;
#3219 = CARTESIAN_POINT ( 'NONE',  ( 1.467888652718972731, -1.850659073900638996, 3.492485675378566246 ) ) ;
#3220 = VERTEX_POINT ( 'NONE', #3147 ) ;
#3221 = CARTESIAN_POINT ( 'NONE',  ( 5.250000000000000000, -27.72916666666666785, -3.031088913245534755 ) ) ;
#3222 = CARTESIAN_POINT ( 'NONE',  ( 1.185285273922203525E-14, -28.71875000068279959, -5.250000000000000000 ) ) ;
#3223 = CARTESIAN_POINT ( 'NONE',  ( -5.114683531250000748, -27.04687500034139802, -6.263680815196995234E-16 ) ) ;
#3224 = VERTEX_POINT ( 'NONE', #5919 ) ;
#3225 = CARTESIAN_POINT ( 'NONE',  ( -5.250000000000000000, -27.00000000000000000, 0.000000000000000000 ) ) ;
#3226 = VERTEX_POINT ( 'NONE', #8762 ) ;
#3227 = EDGE_CURVE ( 'NONE', #4547, #6263, #5645, .T. ) ;
#3228 = CARTESIAN_POINT ( 'NONE',  ( 5.114683531249998971, -29.38020833367473017, 2.952963913586936329 ) ) ;
#3229 = CARTESIAN_POINT ( 'NONE',  ( -2.134148098076978251, -2.049340926099361138, 2.108492589042307408 ) ) ;
#3230 = CARTESIAN_POINT ( 'NONE',  ( 2.625000000000000444, -28.48958333401612819, -4.546633369868303021 ) ) ;
#3231 = DIRECTION ( 'NONE',  ( 0.000000000000000000, 0.000000000000000000, -1.000000000000000000 ) ) ;
#3232 = CARTESIAN_POINT ( 'NONE',  ( 5.114683531250000748, -29.17187500034139802, 0.000000000000000000 ) ) ;
#3233 = SURFACE_STYLE_USAGE ( .BOTH. , #1136 ) ;
#3234 = CARTESIAN_POINT ( 'NONE',  ( -2.033577675846918216E-14, -29.37499999931720396, 5.250000000000000888 ) ) ;
#3235 = CARTESIAN_POINT ( 'NONE',  ( 2.557341765624996821, -27.65104166700806587, 4.429445870380401828 ) ) ;
#3236 = ORIENTED_EDGE ( 'NONE', *, *, #2414, .T. ) ;
#3237 = CYLINDRICAL_SURFACE ( 'NONE', #7792, 4.000000000000000000 ) ;
#3238 = CARTESIAN_POINT ( 'NONE',  ( 2.692658234375002735, -28.27604166632526628, 4.663820869356205101 ) ) ;
#3239 = CARTESIAN_POINT ( 'NONE',  ( -2.692658234374996518, -29.56770833299193413, 4.663820869356208654 ) ) ;
#3240 = CARTESIAN_POINT ( 'NONE',  ( 0.000000000000000000, -20.00000000000000000, 2.500000000000000444 ) ) ;
#3241 = CARTESIAN_POINT ( 'NONE',  ( -3.807688866302469071E-16, -29.92187499965859843, -6.218427825808274356 ) ) ;
#3242 = CARTESIAN_POINT ( 'NONE',  ( 1.638713065079161924, -0.7493409260993607601, 4.007514324621467949 ) ) ;
#3243 = VERTEX_POINT ( 'NONE', #3234 ) ;
#3244 = CARTESIAN_POINT ( 'NONE',  ( 0.000000000000000000, -9.999999999999998224, 0.000000000000000000 ) ) ;
#3245 = CARTESIAN_POINT ( 'NONE',  ( 2.625000000000000444, -28.23958333401612819, -4.546633369868303021 ) ) ;
#3246 = CARTESIAN_POINT ( 'NONE',  ( -2.692658234374996518, -29.06770833299193413, 4.663820869356208654 ) ) ;
#3247 = ADVANCED_FACE ( 'NONE', ( #337 ), #1352, .T. ) ;
#3248 = VERTEX_POINT ( 'NONE', #1742 ) ;
#3249 = CARTESIAN_POINT ( 'NONE',  ( -3.807688866302469071E-16, -27.64062499965859843, -6.218427825808274356 ) ) ;
#3250 = CARTESIAN_POINT ( 'NONE',  ( 2.108492589042352705, -5.550659073900639839, -2.134148098076933397 ) ) ;
#3251 = CYLINDRICAL_SURFACE ( 'NONE', #1777, 5.250000000000000000 ) ;
#3252 =( BOUNDED_CURVE ( )  B_SPLINE_CURVE ( 2, ( #6312, #5045, #1384, #3487, #9106, #4229, #6271, #7152, #7015 ),
 .UNSPECIFIED., .F., .F. ) 
 B_SPLINE_CURVE_WITH_KNOTS ( ( 3, 2, 2, 2, 3 ),
 ( 0.1875000000000000000, 0.1944444444444444475, 0.2083333333333333426, 0.2222222222222222099, 0.2291666666666666574 ),
 .UNSPECIFIED. ) 
 CURVE ( )  GEOMETRIC_REPRESENTATION_ITEM ( )  RATIONAL_B_SPLINE_CURVE ( ( 0.9330127018922194093, 0.9330127018922194093, 1.000000000000000000, 0.8660254037844387076, 1.000000000000000000, 0.8660254037844387076, 1.000000000000000000, 0.9330127018922194093, 0.9330127018922194093 ) ) 
 REPRESENTATION_ITEM ( '' )  );
#3253 = CARTESIAN_POINT ( 'NONE',  ( 0.000000000000000000, -27.00000000000000000, 0.000000000000000000 ) ) ;
#3254 = CARTESIAN_POINT ( 'NONE',  ( 2.624999999999998668, -27.33333333333333570, -4.546633369868303021 ) ) ;
#3255 = CARTESIAN_POINT ( 'NONE',  ( 0.000000000000000000, -30.00000000000000000, 5.250000000000000000 ) ) ;
#3256 = ORIENTED_EDGE ( 'NONE', *, *, #3453, .T. ) ;
#3257 = ITEM_DEFINED_TRANSFORMATION ( 'NONE', 'NONE', #3536,  #888 ) ;
#3258 = CARTESIAN_POINT ( 'NONE',  ( 0.000000000000000000, 70.00000000000000000, 0.000000000000000000 ) ) ;
#3259 = CARTESIAN_POINT ( 'NONE',  ( -2.487701488670255312, -5.249340926099360871, 2.462045979635577808 ) ) ;
#3260 = CARTESIAN_POINT ( 'NONE',  ( 0.000000000000000000, -27.00000000000000000, -5.250000000000000000 ) ) ;
#3261 = CARTESIAN_POINT ( 'NONE',  ( -5.385316468750001029, -28.59895833299193413, -3.109213912904136734 ) ) ;
#3262 = CARTESIAN_POINT ( 'NONE',  ( -0.01814118441313947866, -7.350659073900638774, -3.500000000000000000 ) ) ;
#3263 = ORIENTED_EDGE ( 'NONE', *, *, #248, .F. ) ;
#3264 = CARTESIAN_POINT ( 'NONE',  ( 5.250000000000000000, -27.00000000000000000, 0.000000000000000000 ) ) ;
#3265 = DIRECTION ( 'NONE',  ( -0.000000000000000000, 1.000000000000000000, -0.000000000000000000 ) ) ;
#3266 = CARTESIAN_POINT ( 'NONE',  ( 3.500000000000000000, -3.750659073900639129, -0.01814118441313969030 ) ) ;
#3267 = EDGE_CURVE ( 'NONE', #8580, #2117, #2384, .T. ) ;
#3268 = ORIENTED_EDGE ( 'NONE', *, *, #2410, .F. ) ;
#3269 = AXIS2_PLACEMENT_3D ( 'NONE', #490, #3938, #1750 ) ;
#3270 = CARTESIAN_POINT ( 'NONE',  ( -2.624999999999996891, -28.95833333333333215, 4.546633369868304797 ) ) ;
#3271 = ORIENTED_EDGE ( 'NONE', *, *, #6896, .F. ) ;
#3272 = CARTESIAN_POINT ( 'NONE',  ( -2.557341765625002594, -29.19270833367473017, 4.429445870380399164 ) ) ;
#3273 = CARTESIAN_POINT ( 'NONE',  ( -3.000000000000000444, -0.2493409260993614540, -0.01814118441320822922 ) ) ;
#3274 = AXIS2_PLACEMENT_3D ( 'NONE', #5839, #2310, #117 ) ;
#3275 = PLANE ( 'NONE',  #7022 ) ;
#3276 = CARTESIAN_POINT ( 'NONE',  ( -2.557341765625002594, -28.75520833367473017, 4.429445870380399164 ) ) ;
#3277 = DIRECTION ( 'NONE',  ( 0.000000000000000000, -0.000000000000000000, 1.000000000000000000 ) ) ;
#3278 = EDGE_CURVE ( 'NONE', #5826, #6937, #5346, .T. ) ;
#3279 = COLOUR_RGB ( '',0.8941176470588234615, 0.8941176470588234615, 0.8941176470588234615 ) ;
#3280 = CARTESIAN_POINT ( 'NONE',  ( -2.557341765625002594, -27.44270833367473017, 4.429445870380399164 ) ) ;
#3281 = AXIS2_PLACEMENT_3D ( 'NONE', #7929, #3006, #7182 ) ;
#3282 = CARTESIAN_POINT ( 'NONE',  ( -1.975475456537005874E-15, -28.31249999999999645, 5.250000000000000000 ) ) ;
#3283 = CARTESIAN_POINT ( 'NONE',  ( 5.114683531250000748, -28.42187500034139802, 0.000000000000000000 ) ) ;
#3284 = EDGE_LOOP ( 'NONE', ( #5539, #2644, #1775, #2185, #5030, #4984, #2912, #2342, #7253, #669, #7517, #1675, #6620, #2577, #8652, #4081, #8834, #9071, #6380, #9135, #3136, #472, #1799, #3755, #908, #3099, #2894, #3038 ) ) ;
#3285 = CARTESIAN_POINT ( 'NONE',  ( 2.625000000000002220, -27.91666666666666430, 4.546633369868302132 ) ) ;
#3286 = CARTESIAN_POINT ( 'NONE',  ( 5.385316468750000141, -29.48437499965859843, -6.595110575850215044E-16 ) ) ;
#3287 = CARTESIAN_POINT ( 'NONE',  ( 5.385316468749999252, -29.71354166632527338, -3.109213912904138954 ) ) ;
#3288 = DIRECTION ( 'NONE',  ( 0.000000000000000000, 0.000000000000000000, 1.000000000000000000 ) ) ;
#3289 = CARTESIAN_POINT ( 'NONE',  ( 1.142306659890740623E-15, -29.54687499965859843, 6.218427825808274356 ) ) ;
#3290 = CARTESIAN_POINT ( 'NONE',  ( 0.01814118441321938349, -6.249340926099361759, -4.000000000000000000 ) ) ;
#3291 = ORIENTED_EDGE ( 'NONE', *, *, #5944, .T. ) ;
#3292=STYLED_ITEM('',(#9204),#2131);
#3293 = FACE_OUTER_BOUND ( 'NONE', #1772, .T. ) ;
#3294 = CARTESIAN_POINT ( 'NONE',  ( 2.624999999999996891, -27.82291666734946389, 4.546633369868304797 ) ) ;
#3295 = CARTESIAN_POINT ( 'NONE',  ( -2.692658234375000514, -29.65104166632526983, -4.663820869356205989 ) ) ;
#3296 = ORIENTED_EDGE ( 'NONE', *, *, #3861, .F. ) ;
#3297 = MECHANICAL_DESIGN_GEOMETRIC_PRESENTATION_REPRESENTATION (  '', ( #8174 ), #4159 ) ;
#3298 = CARTESIAN_POINT ( 'NONE',  ( 5.385316468749999252, -28.93229166632526983, -3.109213912904138954 ) ) ;
#3299 = CARTESIAN_POINT ( 'NONE',  ( -2.108492589042352261, -6.350659073900638774, 2.134148098076933397 ) ) ;
#3300 = CARTESIAN_POINT ( 'NONE',  ( -5.250000000000000000, -27.18749999931720396, 0.000000000000000000 ) ) ;
#3301 = ADVANCED_FACE ( 'NONE', ( #4714 ), #742, .T. ) ;
#3302 = FACE_OUTER_BOUND ( 'NONE', #6606, .T. ) ;
#3303 = FACE_OUTER_BOUND ( 'NONE', #6297, .T. ) ;
#3304 = VERTEX_POINT ( 'NONE', #6759 ) ;
#3305 = APPLICATION_PROTOCOL_DEFINITION ( 'draft international standard', 'automotive_design', 1998, #525 ) ;
#3306 = CARTESIAN_POINT ( 'NONE',  ( -5.385316468749998364, -30.05729166632526628, 3.109213912904140287 ) ) ;
#3307 = CARTESIAN_POINT ( 'NONE',  ( -3.492485675378536047, -6.549340926099363358, -1.467888652719048670 ) ) ;
#3308 =( BOUNDED_CURVE ( )  B_SPLINE_CURVE ( 2, ( #6616, #2390, #5121, #6517, #5171, #1692, #4532, #8013, #1740 ),
 .UNSPECIFIED., .F., .T. ) 
 B_SPLINE_CURVE_WITH_KNOTS ( ( 3, 2, 2, 2, 3 ),
 ( 0.4791666666666666852, 0.4861111111111111049, 0.5000000000000000000, 0.5138888888888888395, 0.5208333333333332593 ),
 .UNSPECIFIED. ) 
 CURVE ( )  GEOMETRIC_REPRESENTATION_ITEM ( )  RATIONAL_B_SPLINE_CURVE ( ( 0.9330127018922194093, 0.9330127018922196314, 1.000000000000000000, 0.8660254037844387076, 1.000000000000000000, 0.8660254037844387076, 1.000000000000000000, 0.9330127018922198534, 0.9330127018922192983 ) ) 
 REPRESENTATION_ITEM ( '' )  );
#3309 = DIRECTION ( 'NONE',  ( 0.000000000000000000, 0.000000000000000000, 1.000000000000000000 ) ) ;
#3310 = CARTESIAN_POINT ( 'NONE',  ( 5.385316468750001029, -28.72395833299193413, 3.109213912904135846 ) ) ;
#3311 = CARTESIAN_POINT ( 'NONE',  ( -1.431606283892693066, -1.650659073900638818, 3.507514324621434199 ) ) ;
#3312 = VERTEX_POINT ( 'NONE', #7463 ) ;
#3313 = CARTESIAN_POINT ( 'NONE',  ( 1.406733260263391960, -29.05133545031537068, 5.250000000000000000 ) ) ;
#3314 = DIRECTION ( 'NONE',  ( -0.000000000000000000, -1.000000000000000000, -0.000000000000000000 ) ) ;
#3315 = CARTESIAN_POINT ( 'NONE',  ( 0.000000000000000000, -20.00000000000000000, 0.000000000000000000 ) ) ;
#3316 = EDGE_CURVE ( 'NONE', #845, #183, #5503, .T. ) ;
#3317 = ORIENTED_EDGE ( 'NONE', *, *, #435, .T. ) ;
#3318 =( NAMED_UNIT ( * ) PLANE_ANGLE_UNIT ( ) SI_UNIT ( $, .RADIAN. ) );
#3319 = CARTESIAN_POINT ( 'NONE',  ( -2.624999999999996891, -28.45833333333333215, 4.546633369868304797 ) ) ;
#3320 = CIRCLE ( 'NONE', #780, 2.499999999999999556 ) ;
#3321 = ORIENTED_EDGE ( 'NONE', *, *, #8037, .T. ) ;
#3322 = CARTESIAN_POINT ( 'NONE',  ( 5.114683531250000748, -29.58854166700806232, -2.952963913586932776 ) ) ;
#3323 = CARTESIAN_POINT ( 'NONE',  ( 0.01814118441320878086, -4.649340926099361226, -3.000000000000000444 ) ) ;
#3324 = CYLINDRICAL_SURFACE ( 'NONE', #1239, 5.250000000000000000 ) ;
#3325 = CARTESIAN_POINT ( 'NONE',  ( 5.114683531250000748, -27.92187500034139802, 0.000000000000000000 ) ) ;
#3326 = FILL_AREA_STYLE ('',( #7508 ) ) ;
#3327 = CARTESIAN_POINT ( 'NONE',  ( -1.925759277493323207, -9.035843541029837430E-14, 2.922632427747480222 ) ) ;
#3328 = CARTESIAN_POINT ( 'NONE',  ( 5.114683531249999859, -27.08854166700806232, -2.952963913586932776 ) ) ;
#3329 = CARTESIAN_POINT ( 'NONE',  ( 2.033577675846918216E-14, -27.06250000000000355, 5.250000000000000888 ) ) ;
#3330 = CARTESIAN_POINT ( 'NONE',  ( -5.114683531250000748, -29.29687500034139802, -6.263680815196995234E-16 ) ) ;
#3331 = EDGE_CURVE ( 'NONE', #2547, #3693, #1127, .T. ) ;
#3332 =( BOUNDED_CURVE ( )  B_SPLINE_CURVE ( 2, ( #7928, #3054, #3602, #7136, #5074, #6427, #7271, #1595, #4486 ),
 .UNSPECIFIED., .F., .F. ) 
 B_SPLINE_CURVE_WITH_KNOTS ( ( 3, 2, 2, 2, 3 ),
 ( 0.2708333333333333703, 0.2777777777777777901, 0.2916666666666666852, 0.3055555555555555802, 0.3125000000000000000 ),
 .UNSPECIFIED. ) 
 CURVE ( )  GEOMETRIC_REPRESENTATION_ITEM ( )  RATIONAL_B_SPLINE_CURVE ( ( 0.9330127018922194093, 0.9330127018922196314, 1.000000000000000000, 0.8660254037844387076, 1.000000000000000000, 0.8660254037844387076, 1.000000000000000000, 0.9330127018922194093, 0.9330127018922194093 ) ) 
 REPRESENTATION_ITEM ( '' )  );
#3333 = FACE_BOUND ( 'NONE', #830, .T. ) ;
#3334 = CARTESIAN_POINT ( 'NONE',  ( 5.385316468749999252, -28.21354166632526628, -3.109213912904138954 ) ) ;
#3335 = CARTESIAN_POINT ( 'NONE',  ( -5.250000000000000000, -29.15625000068279604, -6.429395695523604153E-16 ) ) ;
#3336 = CIRCLE ( 'NONE', #7185, 4.250000000000000000 ) ;
#3337 = LINE ( 'NONE', #6211, #5187 ) ;
#3338 = CARTESIAN_POINT ( 'NONE',  ( 1.142306659890740623E-15, -30.04687499965860198, 6.218427825808274356 ) ) ;
#3339 = CARTESIAN_POINT ( 'NONE',  ( -2.462045979635576920, -3.249340926099361315, -2.487701488670255756 ) ) ;
#3340 = CARTESIAN_POINT ( 'NONE',  ( 3.992485675378533383, -7.349340926099363180, 1.674995433905599462 ) ) ;
#3341 = VERTEX_POINT ( 'NONE', #6708 ) ;
#3342 = CARTESIAN_POINT ( 'NONE',  ( 5.250000000000000000, -28.37500000000000000, -6.429395695523604153E-16 ) ) ;
#3343 = CARTESIAN_POINT ( 'NONE',  ( -2.625000000000002220, -28.61458333401612819, 4.546633369868302132 ) ) ;
#3344 = CARTESIAN_POINT ( 'NONE',  ( -5.385316468749998364, -29.83854166632526628, 3.109213912904140287 ) ) ;
#3345 = EDGE_LOOP ( 'NONE', ( #3041, #3724, #5877, #2966 ) ) ;
#3346 = CARTESIAN_POINT ( 'NONE',  ( -5.385316468749998364, -28.05729166632526272, 3.109213912904140287 ) ) ;
#3347 = CARTESIAN_POINT ( 'NONE',  ( 2.487701488670203354, -3.550659073900638951, 2.462045979635629323 ) ) ;
#3348 = CARTESIAN_POINT ( 'NONE',  ( 1.406733260263394625, -29.72991455036742536, -5.250000000000000000 ) ) ;
#3349 = EDGE_CURVE ( 'NONE', #5259, #627, #5870, .T. ) ;
#3350 = CARTESIAN_POINT ( 'NONE',  ( 0.000000000000000000, -27.00000000000000000, 0.000000000000000000 ) ) ;
#3351 = CARTESIAN_POINT ( 'NONE',  ( 0.000000000000000000, 69.99999999999998579, 6.250000000000000000 ) ) ;
#3352 = CARTESIAN_POINT ( 'NONE',  ( 3.492485675378535603, -7.349340926099362292, 1.467888652719046672 ) ) ;
#3353 = CARTESIAN_POINT ( 'NONE',  ( -1.000000000000000000, -29.00000000000000355, -3.048902179152658931 ) ) ;
#3354 = CARTESIAN_POINT ( 'NONE',  ( 0.000000000000000000, -29.87813065659485190, 0.000000000000000000 ) ) ;
#3355 = PRODUCT_CONTEXT ( 'NONE', #3383, 'mechanical' ) ;
#3356 = CARTESIAN_POINT ( 'NONE',  ( 2.692658234375002735, -29.24479166632526983, 4.663820869356205101 ) ) ;
#3357 = CARTESIAN_POINT ( 'NONE',  ( -2.462045979635576920, -6.449340926099361937, -2.487701488670255756 ) ) ;
#3358 = CARTESIAN_POINT ( 'NONE',  ( 5.250000000000000000, -28.56249999931720396, -6.429395695523604153E-16 ) ) ;
#3359 = CARTESIAN_POINT ( 'NONE',  ( 5.385316468750001029, -29.22395833299193413, 3.109213912904135846 ) ) ;
#3360 = CARTESIAN_POINT ( 'NONE',  ( -1.431606283892693066, -4.850659073900638774, 3.507514324621434199 ) ) ;
#3361 = EDGE_LOOP ( 'NONE', ( #541, #7887, #9182, #3588 ) ) ;
#3362 = CARTESIAN_POINT ( 'NONE',  ( 0.000000000000000000, -20.00000000000000000, -1.499999999999999778 ) ) ;
#3363 = DIRECTION ( 'NONE',  ( 0.000000000000000000, 1.000000000000000000, 0.000000000000000000 ) ) ;
#3364 = CARTESIAN_POINT ( 'NONE',  ( 3.492485675378566690, -5.450659073900639306, -1.467888652718972287 ) ) ;
#3365 = VERTEX_POINT ( 'NONE', #5406 ) ;
#3366 = CARTESIAN_POINT ( 'NONE',  ( 2.625000000000002220, -27.91666666666666430, 4.546633369868302132 ) ) ;
#3367 = CARTESIAN_POINT ( 'NONE',  ( -5.114683531250000748, -28.00520833367473017, -2.952963913586935440 ) ) ;
#3368 = CARTESIAN_POINT ( 'NONE',  ( -3.500000000000000000, -8.249340926099360871, -0.01814118441321344033 ) ) ;
#3369 = FACE_OUTER_BOUND ( 'NONE', #63, .T. ) ;
#3370 = CARTESIAN_POINT ( 'NONE',  ( 5.114683531250000748, -27.67187500034139802, 0.000000000000000000 ) ) ;
#3371 = CARTESIAN_POINT ( 'NONE',  ( -1.406733260263394625, -29.23883544963257464, -5.250000000000000000 ) ) ;
#3372 = CARTESIAN_POINT ( 'NONE',  ( -2.557341765625002594, -29.75520833367473017, 4.429445870380399164 ) ) ;
#3373 = CARTESIAN_POINT ( 'NONE',  ( 2.624999999999996891, -27.04166666666666430, 4.546633369868304797 ) ) ;
#3374 = CARTESIAN_POINT ( 'NONE',  ( 2.557341765625000818, -28.38020833367473017, -4.429445870380400052 ) ) ;
#3375 = LINE ( 'NONE', #3507, #8155 ) ;
#3376 = CARTESIAN_POINT ( 'NONE',  ( -5.385316468750000141, -29.10937499965859843, 0.000000000000000000 ) ) ;
#3377 = CARTESIAN_POINT ( 'NONE',  ( -5.385316468750001029, -29.88020833299193413, -3.109213912904136734 ) ) ;
#3378 = CARTESIAN_POINT ( 'NONE',  ( 0.000000000000000000, 79.00000000000001421, 0.000000000000000000 ) ) ;
#3379 = CARTESIAN_POINT ( 'NONE',  ( -5.385316468750001029, -29.13020833299193058, -3.109213912904136734 ) ) ;
#3380 = CARTESIAN_POINT ( 'NONE',  ( 1.467888652719048226, -6.149340926099360338, -3.492485675378536047 ) ) ;
#3381 = CARTESIAN_POINT ( 'NONE',  ( -2.841254879263533262, -5.249340926099361759, 2.815599370228847764 ) ) ;
#3382 = ORIENTED_EDGE ( 'NONE', *, *, #4776, .T. ) ;
#3383 = APPLICATION_CONTEXT ( 'automotive_design' ) ;
#3384 = DIRECTION ( 'NONE',  ( 0.000000000000000000, 1.000000000000000000, 0.000000000000000000 ) ) ;
#3385 = CARTESIAN_POINT ( 'NONE',  ( -2.625000000000002220, -28.11458333401612819, 4.546633369868302132 ) ) ;
#3386 = CARTESIAN_POINT ( 'NONE',  ( 5.385316468750001029, -29.00520833299193413, 3.109213912904135846 ) ) ;
#3387 =( BOUNDED_CURVE ( )  B_SPLINE_CURVE ( 2, ( #8243, #3313, #4701, #3407, #9068, #4188, #3492, #7021, #1350 ),
 .UNSPECIFIED., .F., .T. ) 
 B_SPLINE_CURVE_WITH_KNOTS ( ( 3, 2, 2, 2, 3 ),
 ( 0.3125000000000000000, 0.3194444444444444198, 0.3333333333333333148, 0.3472222222222222099, 0.3541666666666666297 ),
 .UNSPECIFIED. ) 
 CURVE ( )  GEOMETRIC_REPRESENTATION_ITEM ( )  RATIONAL_B_SPLINE_CURVE ( ( 0.9330127018922194093, 0.9330127018922194093, 1.000000000000000000, 0.8660254037844387076, 1.000000000000000000, 0.8660254037844387076, 1.000000000000000000, 0.9330127018922196314, 0.9330127018922194093 ) ) 
 REPRESENTATION_ITEM ( '' )  );
#3388 =( GEOMETRIC_REPRESENTATION_CONTEXT ( 3 ) GLOBAL_UNCERTAINTY_ASSIGNED_CONTEXT ( ( #8034 ) ) GLOBAL_UNIT_ASSIGNED_CONTEXT ( ( #8657, #2288, #11 ) ) REPRESENTATION_CONTEXT ( 'NONE', 'WORKASPACE' ) );
#3389 = EDGE_CURVE ( 'NONE', #7114, #2434, #6159, .T. ) ;
#3390 = ORIENTED_EDGE ( 'NONE', *, *, #2994, .F. ) ;
#3391 = CARTESIAN_POINT ( 'NONE',  ( 2.692658234375002735, -27.74479166632526628, 4.663820869356205101 ) ) ;
#3392 = CARTESIAN_POINT ( 'NONE',  ( 1.224499502706142273, -7.250659073900640905, -3.007514324621435531 ) ) ;
#3393 = DIRECTION ( 'NONE',  ( 0.000000000000000000, 1.000000000000000000, 0.000000000000000000 ) ) ;
#3394 = EDGE_CURVE ( 'NONE', #2074, #4147, #1526, .T. ) ;
#3395 = DIRECTION ( 'NONE',  ( 0.000000000000000000, -0.000000000000000000, 1.000000000000000000 ) ) ;
#3396 = CARTESIAN_POINT ( 'NONE',  ( 0.000000000000000000, 76.00000000000000000, 0.000000000000000000 ) ) ;
#3397 = CARTESIAN_POINT ( 'NONE',  ( -2.487701488670255312, -6.849340926099361404, 2.462045979635577808 ) ) ;
#3398 = CARTESIAN_POINT ( 'NONE',  ( 5.114683531250000748, -29.60937500034139802, 0.000000000000000000 ) ) ;
#3399 = CARTESIAN_POINT ( 'NONE',  ( 2.624999999999996891, -27.57291666734946389, 4.546633369868304797 ) ) ;
#3400 = PRODUCT_CONTEXT ( 'NONE', #525, 'mechanical' ) ;
#3401 = CARTESIAN_POINT ( 'NONE',  ( 1.638713065079247855, -4.050659073900639839, -4.007514324621431534 ) ) ;
#3402 = CARTESIAN_POINT ( 'NONE',  ( -5.385316468750001029, -29.59895833299193413, -3.109213912904136734 ) ) ;
#3403 = CARTESIAN_POINT ( 'NONE',  ( -2.487701488670255312, -3.649340926099361226, 2.462045979635577808 ) ) ;
#3404 = CYLINDRICAL_SURFACE ( 'NONE', #8453, 5.250000000000000000 ) ;
#3405 = CARTESIAN_POINT ( 'NONE',  ( -5.385316468750001029, -29.09895833299193058, -3.109213912904136734 ) ) ;
#3406 = CARTESIAN_POINT ( 'NONE',  ( -4.000000000000000000, -4.550659073900638951, 0.01814118441313491634 ) ) ;
#3407 = CARTESIAN_POINT ( 'NONE',  ( 5.249999999999997335, -29.02083333333332860, 3.031088913245538308 ) ) ;
#3408 = FACE_OUTER_BOUND ( 'NONE', #378, .T. ) ;
#3409 = AXIS2_PLACEMENT_3D ( 'NONE', #1746, #6762, #2541 ) ;
#3410 = ORIENTED_EDGE ( 'NONE', *, *, #144, .F. ) ;
#3411 = CARTESIAN_POINT ( 'NONE',  ( -5.249999999999999112, -28.72916666666666785, 3.031088913245538308 ) ) ;
#3412 = CARTESIAN_POINT ( 'NONE',  ( -5.114683531250000748, -27.75520833367473017, -2.952963913586935440 ) ) ;
#3413 = CARTESIAN_POINT ( 'NONE',  ( 2.108492589042352705, -2.350659073900639218, -2.134148098076933397 ) ) ;
#3414 = CARTESIAN_POINT ( 'NONE',  ( 0.000000000000000000, -27.00000000000000000, -5.250000000000000000 ) ) ;
#3415 = CARTESIAN_POINT ( 'NONE',  ( 2.557341765624996821, -27.96354166700806587, 4.429445870380401828 ) ) ;
#3416 = CARTESIAN_POINT ( 'NONE',  ( 2.300847884672513123E-14, -27.21875000068279959, -5.250000000000000000 ) ) ;
#3417 = EDGE_CURVE ( 'NONE', #5951, #7705, #1393, .T. ) ;
#3418 = CARTESIAN_POINT ( 'NONE',  ( -1.084901341431563726E-15, -28.73437500034139802, 5.905927827173866440 ) ) ;
#3419=STYLED_ITEM('',(#9218),#8209);
#3420 =( NAMED_UNIT ( * ) PLANE_ANGLE_UNIT ( ) SI_UNIT ( $, .RADIAN. ) );
#3421 = CARTESIAN_POINT ( 'NONE',  ( 5.114683531249999859, -29.40104166700806232, -2.952963913586932776 ) ) ;
#3422 = DIRECTION ( 'NONE',  ( 0.000000000000000000, 0.000000000000000000, -1.000000000000000000 ) ) ;
#3423 = CARTESIAN_POINT ( 'NONE',  ( -5.250000000000000000, -28.93749999931720396, 0.000000000000000000 ) ) ;
#3424 = CARTESIAN_POINT ( 'NONE',  ( 2.692658234374998738, -29.94270833299193413, -4.663820869356206877 ) ) ;
#3425 = CARTESIAN_POINT ( 'NONE',  ( 1.406733260263391960, -28.83258545099816672, 5.250000000000000000 ) ) ;
#3426 = DIRECTION ( 'NONE',  ( 0.000000000000000000, -1.000000000000000000, 0.000000000000000000 ) ) ;
#3427 = CARTESIAN_POINT ( 'NONE',  ( 3.507514324621465285, -1.149340926099361226, -1.431606283892619125 ) ) ;
#3428 = CARTESIAN_POINT ( 'NONE',  ( 2.815599370228847320, -5.649340926099361226, 2.841254879263533262 ) ) ;
#3429 = VERTEX_POINT ( 'NONE', #5621 ) ;
#3430 = DIRECTION ( 'NONE',  ( -0.8660254037844402619, 0.4999999999999970579, -0.000000000000000000 ) ) ;
#3431 = AXIS2_PLACEMENT_3D ( 'NONE', #1638, #6419, #57 ) ;
#3432 = CARTESIAN_POINT ( 'NONE',  ( 5.114683531249999859, -29.83854166700806587, -2.952963913586932776 ) ) ;
#3433 = CARTESIAN_POINT ( 'NONE',  ( 5.385316468749999252, -28.96354166632526983, -3.109213912904139399 ) ) ;
#3434 = ORIENTED_EDGE ( 'NONE', *, *, #3202, .F. ) ;
#3435 = CARTESIAN_POINT ( 'NONE',  ( -5.385316468750001029, -29.34895833299193413, -3.109213912904136734 ) ) ;
#3436 = CARTESIAN_POINT ( 'NONE',  ( -2.841254879263473310, -1.150659073900638374, -2.815599370228907716 ) ) ;
#3437 = CARTESIAN_POINT ( 'NONE',  ( 0.000000000000000000, -46.00000000000000000, 0.000000000000000000 ) ) ;
#3438 = CIRCLE ( 'NONE', #1207, 5.250000000000000000 ) ;
#3439 = CARTESIAN_POINT ( 'NONE',  ( -2.625000000000000444, -29.04166666666666785, -4.546633369868303021 ) ) ;
#3440 = DIRECTION ( 'NONE',  ( 0.000000000000000000, -1.000000000000000000, 0.000000000000000000 ) ) ;
#3441 = CARTESIAN_POINT ( 'NONE',  ( 0.000000000000000000, -27.00000000000000000, 0.000000000000000000 ) ) ;
#3442 = CIRCLE ( 'NONE', #8629, 2.499999999999999556 ) ;
#3443 = CARTESIAN_POINT ( 'NONE',  ( -1.084901341431563923E-15, -28.67187500034139802, 5.905927827173866440 ) ) ;
#3444 = LINE ( 'NONE', #5613, #8804 ) ;
#3445 = CARTESIAN_POINT ( 'NONE',  ( -3.500000000000000000, -6.649340926099361226, -0.01814118441321344033 ) ) ;
#3446 = EDGE_CURVE ( 'NONE', #7910, #4820, #8491, .T. ) ;
#3447 = CARTESIAN_POINT ( 'NONE',  ( 0.000000000000000000, -47.00000000000000000, 0.000000000000000000 ) ) ;
#3448 = CARTESIAN_POINT ( 'NONE',  ( -5.385316468749998364, -29.55729166632526983, 3.109213912904140287 ) ) ;
#3449 = CARTESIAN_POINT ( 'NONE',  ( 4.000000000000000000, -2.150659073900639040, -0.01814118441313441674 ) ) ;
#3450 = DIRECTION ( 'NONE',  ( 0.000000000000000000, 1.000000000000000000, 0.000000000000000000 ) ) ;
#3451 = EDGE_LOOP ( 'NONE', ( #4192, #3495, #3053, #5205, #8532, #720 ) ) ;
#3452 = CARTESIAN_POINT ( 'NONE',  ( 5.250000000000000888, -28.14583333333333215, 3.031088913245532979 ) ) ;
#3453 = EDGE_CURVE ( 'NONE', #4194, #6523, #2539, .T. ) ;
#3454 = CARTESIAN_POINT ( 'NONE',  ( -5.114683531250000748, -28.25520833367473017, -2.952963913586935440 ) ) ;
#3455 = CARTESIAN_POINT ( 'NONE',  ( -3.000000000000000444, -6.649340926099362115, -0.01814118441320822922 ) ) ;
#3456 = CARTESIAN_POINT ( 'NONE',  ( -1.084901341431563923E-15, -27.23437500034139802, 5.905927827173866440 ) ) ;
#3457 = CARTESIAN_POINT ( 'NONE',  ( 0.000000000000000000, -30.00000000000000000, 5.250000000000000000 ) ) ;
#3458 = CARTESIAN_POINT ( 'NONE',  ( -2.557341765625002594, -29.25520833367473017, 4.429445870380399164 ) ) ;
#3459 = VECTOR ( 'NONE', #3985, 1000.000000000000000 ) ;
#3460 = DIRECTION ( 'NONE',  ( 0.000000000000000000, 0.000000000000000000, -1.000000000000000000 ) ) ;
#3461 = CARTESIAN_POINT ( 'NONE',  ( 3.616337804771879580E-16, -29.60937500034139447, -5.905927827173866440 ) ) ;
#3462 = CARTESIAN_POINT ( 'NONE',  ( -1.406733260263393293, -28.45758545099816672, -5.250000000000000000 ) ) ;
#3463 = CARTESIAN_POINT ( 'NONE',  ( -2.625000000000000444, -28.72916666598386826, -4.546633369868303021 ) ) ;
#3464 = CARTESIAN_POINT ( 'NONE',  ( -1.467888652719046449, -0.5493409260993611376, 3.492485675378536047 ) ) ;
#3465 = CARTESIAN_POINT ( 'NONE',  ( 1.406733260263391960, -29.58258545099816317, 5.250000000000000000 ) ) ;
#3466 = PLANE ( 'NONE',  #3609 ) ;
#3467 = CARTESIAN_POINT ( 'NONE',  ( -0.01814118441321365544, -0.6493409260993610044, 3.500000000000000000 ) ) ;
#3468 = CARTESIAN_POINT ( 'NONE',  ( -1.674995433905599462, -6.949340926099362825, 3.992485675378533383 ) ) ;
#3469 = AXIS2_PLACEMENT_3D ( 'NONE', #5264, #6756, #3231 ) ;
#3470 = VERTEX_POINT ( 'NONE', #3535 ) ;
#3471 = AXIS2_PLACEMENT_3D ( 'NONE', #1337, #7896, #2214 ) ;
#3472 = CARTESIAN_POINT ( 'NONE',  ( -5.250000000000000888, -26.88541666734946389, 3.031088913245532979 ) ) ;
#3473 = VECTOR ( 'NONE', #6791, 1000.000000000000000 ) ;
#3474 = AXIS2_PLACEMENT_3D ( 'NONE', #3003, #153, #7318 ) ;
#3475 = ORIENTED_EDGE ( 'NONE', *, *, #5195, .T. ) ;
#3476 = CARTESIAN_POINT ( 'NONE',  ( 1.142306659890740623E-15, -29.51562499965859487, 6.218427825808274356 ) ) ;
#3477 = CARTESIAN_POINT ( 'NONE',  ( -2.487701488670202910, -4.350659073900638774, -2.462045979635629767 ) ) ;
#3478 = CARTESIAN_POINT ( 'NONE',  ( -5.249999999999999112, -27.14583333333332860, -3.031088913245536975 ) ) ;
#3479 = EDGE_CURVE ( 'NONE', #7866, #3081, #7126, .T. ) ;
#3480 = VECTOR ( 'NONE', #68, 1000.000000000000000 ) ;
#3481 = DIRECTION ( 'NONE',  ( 0.000000000000000000, -1.000000000000000000, 0.000000000000000000 ) ) ;
#3482 = LINE ( 'NONE', #3615, #4273 ) ;
#3483 = CARTESIAN_POINT ( 'NONE',  ( 1.836970198721029688E-16, -20.00000000000000000, 1.499999999999999778 ) ) ;
#3484 = CARTESIAN_POINT ( 'NONE',  ( -1.084901341431563923E-15, -29.17187500034139802, 5.905927827173866440 ) ) ;
#3485 = DIRECTION ( 'NONE',  ( -0.000000000000000000, -1.000000000000000000, -0.000000000000000000 ) ) ;
#3486 = PRODUCT_DEFINITION ( 'UNKNOWN', '', #2945, #1339 ) ;
#3487 = CARTESIAN_POINT ( 'NONE',  ( 5.249999999999999112, -27.79166666598386826, -3.031088913245536975 ) ) ;
#3488 = CARTESIAN_POINT ( 'NONE',  ( 1.260781871532495657, -6.149340926099362115, -2.992485675378538268 ) ) ;
#3489 = CARTESIAN_POINT ( 'NONE',  ( -2.625000000000002220, -28.11458333401612819, 4.546633369868302132 ) ) ;
#3490 = CARTESIAN_POINT ( 'NONE',  ( -2.692658234375000514, -29.36979166632526983, -4.663820869356205989 ) ) ;
#3491 = CARTESIAN_POINT ( 'NONE',  ( 0.01814118441313467001, -3.350659073900638774, 4.000000000000000000 ) ) ;
#3492 = CARTESIAN_POINT ( 'NONE',  ( 2.625000000000000444, -28.95833333333333215, -4.546633369868303021 ) ) ;
#3493 = FACE_OUTER_BOUND ( 'NONE', #769, .T. ) ;
#3494 = CARTESIAN_POINT ( 'NONE',  ( -3.500000000000000000, -8.000000000000000000, -3.665958595716611867E-14 ) ) ;
#3495 = ORIENTED_EDGE ( 'NONE', *, *, #7243, .T. ) ;
#3496 = CARTESIAN_POINT ( 'NONE',  ( 5.250000000000000000, -29.35416666666666430, -3.031088913245536531 ) ) ;
#3497 = EDGE_CURVE ( 'NONE', #3872, #2716, #1416, .T. ) ;
#3498 = ORIENTED_EDGE ( 'NONE', *, *, #5900, .F. ) ;
#3499 = CARTESIAN_POINT ( 'NONE',  ( -5.114683531250000748, -28.23437500034139447, -6.263680815196995234E-16 ) ) ;
#3500 = CARTESIAN_POINT ( 'NONE',  ( -1.224499502706077880, -7.949340926099362825, -3.007514324621463064 ) ) ;
#3501 = CARTESIAN_POINT ( 'NONE',  ( -2.557341765624999042, -27.33854166700806587, -4.429445870380400052 ) ) ;
#3502 = LINE ( 'NONE', #7825, #9116 ) ;
#3503 = EDGE_CURVE ( 'NONE', #4350, #4963, #7874, .T. ) ;
#3504 = CARTESIAN_POINT ( 'NONE',  ( 5.114683531250000748, -29.40104166700806232, -2.952963913586932776 ) ) ;
#3505 = EDGE_CURVE ( 'NONE', #7184, #8201, #7816, .T. ) ;
#3506 = CARTESIAN_POINT ( 'NONE',  ( -2.557341765624999042, -27.83854166700806587, -4.429445870380400052 ) ) ;
#3507 = CARTESIAN_POINT ( 'NONE',  ( 6.429395695523604153E-16, -27.00000000000000000, 5.250000000000000000 ) ) ;
#3508 = CARTESIAN_POINT ( 'NONE',  ( 2.625000000000002220, -29.85416666598387181, 4.546633369868302132 ) ) ;
#3509 = CYLINDRICAL_SURFACE ( 'NONE', #7625, 5.250000000000000000 ) ;
#3510 =( LENGTH_UNIT ( ) NAMED_UNIT ( * ) SI_UNIT ( .MILLI., .METRE. ) );
#3511 = CARTESIAN_POINT ( 'NONE',  ( 0.000000000000000000, -9.999999999999998224, 4.250000000000000000 ) ) ;
#3512 = CARTESIAN_POINT ( 'NONE',  ( -2.462045979635576920, -1.649340926099361004, -2.487701488670255756 ) ) ;
#3513 = CARTESIAN_POINT ( 'NONE',  ( 0.01814118441321408565, -4.649340926099361226, -3.500000000000000000 ) ) ;
#3514 = ORIENTED_EDGE ( 'NONE', *, *, #6799, .F. ) ;
#3515 = DIRECTION ( 'NONE',  ( 0.000000000000000000, 0.000000000000000000, 1.000000000000000000 ) ) ;
#3516 = CARTESIAN_POINT ( 'NONE',  ( 2.624999999999996891, -27.32291666734946389, 4.546633369868304797 ) ) ;
#3517 = ORIENTED_EDGE ( 'NONE', *, *, #7310, .T. ) ;
#3518 = CARTESIAN_POINT ( 'NONE',  ( 2.692658234374998738, -29.66145833299193413, -4.663820869356206877 ) ) ;
#3519 = CARTESIAN_POINT ( 'NONE',  ( -2.487701488670202910, -5.950659073900639306, -2.462045979635629767 ) ) ;
#3520 = CARTESIAN_POINT ( 'NONE',  ( -2.625000000000002220, -27.08333333333333570, 4.546633369868302132 ) ) ;
#3521 = ORIENTED_EDGE ( 'NONE', *, *, #2354, .F. ) ;
#3522 = EDGE_CURVE ( 'NONE', #8472, #187, #4278, .T. ) ;
#3523 = PRODUCT ( 'dispenser', 'dispenser', '', ( #3355 ) ) ;
#3524 = LINE ( 'NONE', #9099, #1807 ) ;
#3525 = CYLINDRICAL_SURFACE ( 'NONE', #3732, 5.250000000000000000 ) ;
#3526 = EDGE_CURVE ( 'NONE', #2600, #3793, #1951, .T. ) ;
#3527 = FACE_OUTER_BOUND ( 'NONE', #348, .T. ) ;
#3528 = CARTESIAN_POINT ( 'NONE',  ( -2.557341765625002594, -28.69270833367473017, 4.429445870380399164 ) ) ;
#3529 = CARTESIAN_POINT ( 'NONE',  ( 1.975475456537005874E-15, -28.12499999931720041, 5.250000000000000000 ) ) ;
#3530 = DIRECTION ( 'NONE',  ( -0.000000000000000000, 1.000000000000000000, -0.000000000000000000 ) ) ;
#3531 = CARTESIAN_POINT ( 'NONE',  ( -2.992485675378538268, -6.549340926099361582, -1.260781871532495879 ) ) ;
#3532 = CARTESIAN_POINT ( 'NONE',  ( 1.975475456537005874E-15, -29.43750000000000000, 5.249999999999999112 ) ) ;
#3533 = CARTESIAN_POINT ( 'NONE',  ( 5.385316468749999252, -29.68229166632526983, -3.109213912904139399 ) ) ;
#3534 = CARTESIAN_POINT ( 'NONE',  ( 1.674995433905515085, -0.2506590739006385182, 3.992485675378568022 ) ) ;
#3535 = CARTESIAN_POINT ( 'NONE',  ( 0.000000000000000000, -27.00000000000000000, -5.250000000000000000 ) ) ;
#3536 = AXIS2_PLACEMENT_3D ( 'NONE', #4603, #4514, #7391 ) ;
#3537 = ORIENTED_EDGE ( 'NONE', *, *, #6341, .T. ) ;
#3538 =( NAMED_UNIT ( * ) SI_UNIT ( $, .STERADIAN. ) SOLID_ANGLE_UNIT ( ) );
#3539 = CARTESIAN_POINT ( 'NONE',  ( 2.624999999999998668, -29.58333333333333215, -4.546633369868303021 ) ) ;
#3540 = CARTESIAN_POINT ( 'NONE',  ( -5.114683531250000748, -27.98437500034139802, -6.263680815196995234E-16 ) ) ;
#3541 = CARTESIAN_POINT ( 'NONE',  ( 1.224499502706077214, -7.149340926099361226, 3.007514324621463508 ) ) ;
#3542 = CARTESIAN_POINT ( 'NONE',  ( 5.250000000000000000, -29.25000000000000000, 0.000000000000000000 ) ) ;
#3543 = DIRECTION ( 'NONE',  ( 0.000000000000000000, -1.000000000000000000, 0.000000000000000000 ) ) ;
#3544 =( BOUNDED_CURVE ( )  B_SPLINE_CURVE ( 2, ( #6657, #5119, #1690, #1642, #2388, #4481, #6614, #8011, #2338 ),
 .UNSPECIFIED., .F., .T. ) 
 B_SPLINE_CURVE_WITH_KNOTS ( ( 3, 2, 2, 2, 3 ),
 ( 0.3958333333333333703, 0.4027777777777777901, 0.4166666666666666852, 0.4305555555555555802, 0.4375000000000000000 ),
 .UNSPECIFIED. ) 
 CURVE ( )  GEOMETRIC_REPRESENTATION_ITEM ( )  RATIONAL_B_SPLINE_CURVE ( ( 0.9330127018922194093, 0.9330127018922196314, 1.000000000000000000, 0.8660254037844387076, 1.000000000000000000, 0.8660254037844387076, 1.000000000000000000, 0.9330127018922194093, 0.9330127018922194093 ) ) 
 REPRESENTATION_ITEM ( '' )  );
#3545 = CARTESIAN_POINT ( 'NONE',  ( -1.084901341431563726E-15, -28.98437500034139802, 5.905927827173866440 ) ) ;
#3546 =( NAMED_UNIT ( * ) SI_UNIT ( $, .STERADIAN. ) SOLID_ANGLE_UNIT ( ) );
#3547 = CIRCLE ( 'NONE', #7110, 1.500000000000000222 ) ;
#3548 =( REPRESENTATION_RELATIONSHIP ('NONE','NONE', #735, #1697 ) REPRESENTATION_RELATIONSHIP_WITH_TRANSFORMATION ( #3257 )SHAPE_REPRESENTATION_RELATIONSHIP( ) );
#3549 = CARTESIAN_POINT ( 'NONE',  ( -5.114683531249999859, -27.06770833367473017, -2.952963913586935440 ) ) ;
#3550 = CYLINDRICAL_SURFACE ( 'NONE', #4735, 1.499999999999999778 ) ;
#3551 = CARTESIAN_POINT ( 'NONE',  ( -2.624999999999996891, -28.64583333265053611, 4.546633369868304797 ) ) ;
#3552 = CARTESIAN_POINT ( 'NONE',  ( 5.250000000000000888, -27.58333333265053611, 3.031088913245533423 ) ) ;
#3553 = EDGE_CURVE ( 'NONE', #566, #849, #1179, .T. ) ;
#3554 = CARTESIAN_POINT ( 'NONE',  ( -2.074671974031725874, -3.217773792136106728E-17, 2.904849880052185362 ) ) ;
#3555 = DIRECTION ( 'NONE',  ( 1.000000000000000000, 0.000000000000000000, 0.000000000000000000 ) ) ;
#3556 = CARTESIAN_POINT ( 'NONE',  ( 0.01814118441321408565, -6.249340926099360871, -3.500000000000000000 ) ) ;
#3557 = ORIENTED_EDGE ( 'NONE', *, *, #5300, .F. ) ;
#3558 = VECTOR ( 'NONE', #3949, 1000.000000000000000 ) ;
#3559 = DIRECTION ( 'NONE',  ( 0.000000000000000000, 0.000000000000000000, -1.000000000000000000 ) ) ;
#3560 = CARTESIAN_POINT ( 'NONE',  ( -2.557341765624999042, -29.77604166700806232, -4.429445870380400052 ) ) ;
#3561 = ORIENTED_EDGE ( 'NONE', *, *, #1000, .F. ) ;
#3562 = EDGE_LOOP ( 'NONE', ( #4564, #547 ) ) ;
#3563 =( GEOMETRIC_REPRESENTATION_CONTEXT ( 3 ) GLOBAL_UNCERTAINTY_ASSIGNED_CONTEXT ( ( #7291 ) ) GLOBAL_UNIT_ASSIGNED_CONTEXT ( ( #3510, #2026, #623 ) ) REPRESENTATION_CONTEXT ( 'NONE', 'WORKASPACE' ) );
#3564 = CARTESIAN_POINT ( 'NONE',  ( 5.385316468750001029, -29.97395833299194123, 3.109213912904134958 ) ) ;
#3565 = CARTESIAN_POINT ( 'NONE',  ( 2.462045979635629767, -5.550659073900639839, -2.487701488670203354 ) ) ;
#3566 = CARTESIAN_POINT ( 'NONE',  ( 7.041719095097280880E-16, -9.999999999999998224, -5.750000000000000000 ) ) ;
#3567 = CIRCLE ( 'NONE', #2381, 3.999999999999999112 ) ;
#3568 = ORIENTED_EDGE ( 'NONE', *, *, #1863, .T. ) ;
#3569 = DIRECTION ( 'NONE',  ( 0.000000000000000000, 1.000000000000000000, 0.000000000000000000 ) ) ;
#3570 = CARTESIAN_POINT ( 'NONE',  ( 2.033577675846918216E-14, -28.06249999999999645, 5.250000000000000888 ) ) ;
#3571 = CARTESIAN_POINT ( 'NONE',  ( 1.406733260263385521, -28.92633545031537068, 5.250000000000006217 ) ) ;
#3572 = CARTESIAN_POINT ( 'NONE',  ( -5.114683531249999859, -28.25520833367473017, -2.952963913586935440 ) ) ;
#3573 = DIRECTION ( 'NONE',  ( 1.000000000000000000, 0.000000000000000000, 0.000000000000000000 ) ) ;
#3574 = CONTEXT_DEPENDENT_SHAPE_REPRESENTATION ( #2302, #2758 ) ;
#3575 = CARTESIAN_POINT ( 'NONE',  ( 1.406733260263400176, -28.97991455036743247, -5.249999999999997335 ) ) ;
#3576 = CARTESIAN_POINT ( 'NONE',  ( 2.108492589042307408, -2.449340926099361937, 2.134148098076978251 ) ) ;
#3577 = DIRECTION ( 'NONE',  ( 0.000000000000000000, -1.000000000000000000, 0.000000000000000000 ) ) ;
#3578 = CARTESIAN_POINT ( 'NONE',  ( -2.692658234374996518, -28.31770833299193413, 4.663820869356208654 ) ) ;
#3579 = CARTESIAN_POINT ( 'NONE',  ( 3.992485675378568910, -2.250659073900638685, -1.674995433905514863 ) ) ;
#3580 = CIRCLE ( 'NONE', #2095, 4.000000000000000000 ) ;
#3581 = DIRECTION ( 'NONE',  ( 0.000000000000000000, 0.000000000000000000, -1.000000000000000000 ) ) ;
#3582 = CARTESIAN_POINT ( 'NONE',  ( -5.250000000000000888, -26.88541666734946389, 3.031088913245533423 ) ) ;
#3583 = ORIENTED_EDGE ( 'NONE', *, *, #3227, .T. ) ;
#3584 = CARTESIAN_POINT ( 'NONE',  ( 5.250000000000000888, -29.14583333333333925, 3.031088913245532979 ) ) ;
#3585 = VERTEX_POINT ( 'NONE', #7158 ) ;
#3586 = CARTESIAN_POINT ( 'NONE',  ( 1.142306659890740623E-15, -27.51562499965859843, 6.218427825808274356 ) ) ;
#3587 = CARTESIAN_POINT ( 'NONE',  ( -0.01814118441314477650, -0.9506590739006395285, -3.000000000000000444 ) ) ;
#3588 = ORIENTED_EDGE ( 'NONE', *, *, #4748, .F. ) ;
#3589 = CARTESIAN_POINT ( 'NONE',  ( 2.625000000000000444, -28.95833333333333215, -4.546633369868303021 ) ) ;
#3590 = FACE_OUTER_BOUND ( 'NONE', #6790, .T. ) ;
#3591 = ADVANCED_FACE ( 'NONE', ( #3629 ), #6451, .T. ) ;
#3592 = CARTESIAN_POINT ( 'NONE',  ( -5.114683531250000748, -27.79687500034139802, -6.263680815196995234E-16 ) ) ;
#3593 = CARTESIAN_POINT ( 'NONE',  ( 2.557341765624996821, -27.96354166700806587, 4.429445870380401828 ) ) ;
#3594 = DIRECTION ( 'NONE',  ( 0.000000000000000000, 1.000000000000000000, 0.000000000000000000 ) ) ;
#3595 =( BOUNDED_CURVE ( )  B_SPLINE_CURVE ( 2, ( #58, #5594, #7128, #14, #751, #3552, #2817, #9168, #2862 ),
 .UNSPECIFIED., .F., .T. ) 
 B_SPLINE_CURVE_WITH_KNOTS ( ( 3, 2, 2, 2, 3 ),
 ( 0.1041666666666666713, 0.1111111111111111049, 0.1250000000000000000, 0.1388888888888888951, 0.1458333333333333426 ),
 .UNSPECIFIED. ) 
 CURVE ( )  GEOMETRIC_REPRESENTATION_ITEM ( )  RATIONAL_B_SPLINE_CURVE ( ( 0.9330127018922194093, 0.9330127018922194093, 1.000000000000000000, 0.8660254037844387076, 1.000000000000000000, 0.8660254037844387076, 1.000000000000000000, 0.9330127018922194093, 0.9330127018922194093 ) ) 
 REPRESENTATION_ITEM ( '' )  );
#3596 = CARTESIAN_POINT ( 'NONE',  ( -1.000000000000000000, -32.99988997691444581, -2.732192653641477786 ) ) ;
#3597 = CARTESIAN_POINT ( 'NONE',  ( -3.750000000000003109, -1.355252715626601757E-17, 0.3087531627310677318 ) ) ;
#3598 = CARTESIAN_POINT ( 'NONE',  ( 0.000000000000000000, -9.999999999999998224, 5.250000000000000000 ) ) ;
#3599 = CARTESIAN_POINT ( 'NONE',  ( -5.114683531250000748, -29.52604166700806232, 2.952963913586931888 ) ) ;
#3600 = CARTESIAN_POINT ( 'NONE',  ( -2.462045979635576920, -6.449340926099361937, -2.487701488670255756 ) ) ;
#3601 = ORIENTED_EDGE ( 'NONE', *, *, #7269, .F. ) ;
#3602 = CARTESIAN_POINT ( 'NONE',  ( 2.624999999999998668, -28.02083333265053255, -4.546633369868303021 ) ) ;
#3603 = CARTESIAN_POINT ( 'NONE',  ( 5.250000000000000888, -29.14583333333333925, 3.031088913245533423 ) ) ;
#3604 = CARTESIAN_POINT ( 'NONE',  ( 5.250000000000000000, -27.28125000068279604, 0.000000000000000000 ) ) ;
#3605 = ORIENTED_EDGE ( 'NONE', *, *, #2128, .F. ) ;
#3606 = VERTEX_POINT ( 'NONE', #2274 ) ;
#3607 = CARTESIAN_POINT ( 'NONE',  ( 1.142306659890740623E-15, -29.76562499965859843, 6.218427825808274356 ) ) ;
#3608 = CARTESIAN_POINT ( 'NONE',  ( 1.638713065079247855, -0.8506590739006385515, -4.007514324621431534 ) ) ;
#3609 = AXIS2_PLACEMENT_3D ( 'NONE', #9087, #2065, #5021 ) ;
#3610 = CARTESIAN_POINT ( 'NONE',  ( 2.300847884672513123E-14, -27.68750000000000355, -5.250000000000000000 ) ) ;
#3611 = CIRCLE ( 'NONE', #3471, 2.549999999999999822 ) ;
#3612 = EDGE_LOOP ( 'NONE', ( #1079, #1555, #5444, #1413 ) ) ;
#3613 = CARTESIAN_POINT ( 'NONE',  ( -5.250000000000000888, -27.60416666666666430, 3.031088913245533423 ) ) ;
#3614 = VECTOR ( 'NONE', #8286, 1000.000000000000000 ) ;
#3615 = CARTESIAN_POINT ( 'NONE',  ( 0.000000000000000000, 70.00000000000000000, -1.500000000000000222 ) ) ;
#3616 = CARTESIAN_POINT ( 'NONE',  ( 2.033577675846918216E-14, -27.84375000068279959, 5.250000000000000888 ) ) ;
#3617 = AXIS2_PLACEMENT_3D ( 'NONE', #7120, #3543, #7687 ) ;
#3618 = CARTESIAN_POINT ( 'NONE',  ( -2.557341765625002594, -27.19270833367473017, 4.429445870380399164 ) ) ;
#3619 = DIRECTION ( 'NONE',  ( 0.000000000000000000, 1.000000000000000000, 0.000000000000000000 ) ) ;
#3620 = CARTESIAN_POINT ( 'NONE',  ( 0.000000000000000000, 74.00000000000001421, 0.000000000000000000 ) ) ;
#3621 = ADVANCED_FACE ( 'NONE', ( #5101 ), #5335, .F. ) ;
#3622 = CARTESIAN_POINT ( 'NONE',  ( 1.260781871532495657, -4.549340926099363358, -2.992485675378538268 ) ) ;
#3623 = CARTESIAN_POINT ( 'NONE',  ( -3.500000000000000000, -8.000000000000000000, -3.665958595716611867E-14 ) ) ;
#3624 =( BOUNDED_CURVE ( )  B_SPLINE_CURVE ( 2, ( #3529, #7014, #2750, #8375, #2130, #2839, #6971, #5571, #9059 ),
 .UNSPECIFIED., .F., .T. ) 
 B_SPLINE_CURVE_WITH_KNOTS ( ( 3, 2, 2, 2, 3 ),
 ( 0.3125000000000000000, 0.3194444444444444198, 0.3333333333333333148, 0.3472222222222222099, 0.3541666666666666852 ),
 .UNSPECIFIED. ) 
 CURVE ( )  GEOMETRIC_REPRESENTATION_ITEM ( )  RATIONAL_B_SPLINE_CURVE ( ( 0.9330127018922194093, 0.9330127018922194093, 1.000000000000000000, 0.8660254037844387076, 1.000000000000000000, 0.8660254037844387076, 1.000000000000000000, 0.9330127018922190762, 0.9330127018922194093 ) ) 
 REPRESENTATION_ITEM ( '' )  );
#3625 = CARTESIAN_POINT ( 'NONE',  ( -5.385316468750000141, -27.85937499965860198, 0.000000000000000000 ) ) ;
#3626 = CARTESIAN_POINT ( 'NONE',  ( -4.000000000000000000, -7.750659073900639129, 0.01814118441313491634 ) ) ;
#3627 = VECTOR ( 'NONE', #7104, 1000.000000000000114 ) ;
#3628 = CARTESIAN_POINT ( 'NONE',  ( 0.000000000000000000, -9.999999999999998224, 0.000000000000000000 ) ) ;
#3629 = FACE_OUTER_BOUND ( 'NONE', #2446, .T. ) ;
#3630 = ORIENTED_EDGE ( 'NONE', *, *, #901, .F. ) ;
#3631 = CARTESIAN_POINT ( 'NONE',  ( 1.142306659890740623E-15, -27.51562499965859843, 6.218427825808274356 ) ) ;
#3632 = ORIENTED_EDGE ( 'NONE', *, *, #8113, .T. ) ;
#3633 = CARTESIAN_POINT ( 'NONE',  ( -5.385316468750001029, -27.34895833299193768, -3.109213912904136734 ) ) ;
#3634 = CARTESIAN_POINT ( 'NONE',  ( 2.462045979635629767, -0.7506590739006389068, -2.487701488670203354 ) ) ;
#3635 = ADVANCED_BREP_SHAPE_REPRESENTATION ( '', ( #5214, #888 ), #6484 ) ;
#3636 = VERTEX_POINT ( 'NONE', #2321 ) ;
#3637 = CARTESIAN_POINT ( 'NONE',  ( -5.250000000000000000, -28.62499999999999645, -6.429395695523604153E-16 ) ) ;
#3638 = DIRECTION ( 'NONE',  ( 0.000000000000000000, 1.000000000000000000, 0.000000000000000000 ) ) ;
#3639 = CARTESIAN_POINT ( 'NONE',  ( 5.114683531250000748, -27.40104166700806587, -2.952963913586932776 ) ) ;
#3640 = CARTESIAN_POINT ( 'NONE',  ( -5.114683531249999859, -28.06770833367473017, -2.952963913586935440 ) ) ;
#3641 = CARTESIAN_POINT ( 'NONE',  ( 5.250000000000000000, -30.06249999931720041, -6.429395695523604153E-16 ) ) ;
#3642 = LINE ( 'NONE', #2951, #4509 ) ;
#3643 = CARTESIAN_POINT ( 'NONE',  ( 0.000000000000000000, 70.00000000000000000, 0.000000000000000000 ) ) ;
#3644 = CARTESIAN_POINT ( 'NONE',  ( -2.625000000000000444, -28.29166666666666785, -4.546633369868303021 ) ) ;
#3645 = CARTESIAN_POINT ( 'NONE',  ( 1.431606283892619125, -7.149340926099362115, 3.507514324621464397 ) ) ;
#3646 = CARTESIAN_POINT ( 'NONE',  ( 1.467888652719048226, -7.749340926099361759, -3.492485675378536047 ) ) ;
#3647 = ORIENTED_EDGE ( 'NONE', *, *, #7606, .F. ) ;
#3648 = CARTESIAN_POINT ( 'NONE',  ( -1.406733260263390628, -28.60491455036742892, 5.250000000000001776 ) ) ;
#3649 = CARTESIAN_POINT ( 'NONE',  ( -1.084901341431563923E-15, -28.67187500034139802, 5.905927827173866440 ) ) ;
#3650 = ORIENTED_EDGE ( 'NONE', *, *, #4456, .F. ) ;
#3651 = EDGE_LOOP ( 'NONE', ( #5998, #1417, #2871 ) ) ;
#3652 = CARTESIAN_POINT ( 'NONE',  ( 5.250000000000000000, -29.62500000000000000, -6.429395695523604153E-16 ) ) ;
#3653 = CARTESIAN_POINT ( 'NONE',  ( 5.385316468750000141, -27.23437499965860198, -6.595110575850215044E-16 ) ) ;
#3654 = CARTESIAN_POINT ( 'NONE',  ( -4.007514324621431534, -7.650659073900639484, -1.638713065079248521 ) ) ;
#3655 = ORIENTED_EDGE ( 'NONE', *, *, #8343, .F. ) ;
#3656 = CARTESIAN_POINT ( 'NONE',  ( -1.406733260263389518, -27.98883544963257464, -5.250000000000001776 ) ) ;
#3657 = CARTESIAN_POINT ( 'NONE',  ( -2.624999999999998668, -29.19791666734946389, -4.546633369868303021 ) ) ;
#3658 = EDGE_CURVE ( 'NONE', #7146, #3793, #531, .T. ) ;
#3659 = CARTESIAN_POINT ( 'NONE',  ( 1.975475456537005874E-15, -27.37499999931720041, 5.250000000000000000 ) ) ;
#3660 = UNCERTAINTY_MEASURE_WITH_UNIT (LENGTH_MEASURE( 1.000000000000000082E-05 ), #4661, 'distance_accuracy_value', 'NONE');
#3661 = CARTESIAN_POINT ( 'NONE',  ( 5.114683531249999859, -29.90104166700806232, -2.952963913586932776 ) ) ;
#3662 = CARTESIAN_POINT ( 'NONE',  ( 2.462045979635577364, -0.8493409260993610710, 2.487701488670255312 ) ) ;
#3663 = PLANE ( 'NONE',  #945 ) ;
#3664 = CARTESIAN_POINT ( 'NONE',  ( -2.992485675378538268, -1.749340926099361981, -1.260781871532495879 ) ) ;
#3665 = EDGE_CURVE ( 'NONE', #8002, #2547, #2126, .T. ) ;
#3666 = DIRECTION ( 'NONE',  ( 0.000000000000000000, 0.000000000000000000, 1.000000000000000000 ) ) ;
#3667 = CARTESIAN_POINT ( 'NONE',  ( -5.385316468749998364, -28.58854166632526983, 3.109213912904140287 ) ) ;
#3668 = CARTESIAN_POINT ( 'NONE',  ( -2.841254879263533262, -2.049340926099361138, 2.815599370228847764 ) ) ;
#3669 = EDGE_CURVE ( 'NONE', #6874, #296, #8611, .T. ) ;
#3670 = DIRECTION ( 'NONE',  ( -0.000000000000000000, -1.000000000000000000, -0.000000000000000000 ) ) ;
#3671 = CARTESIAN_POINT ( 'NONE',  ( 0.000000000000000000, 70.00000000000000000, 0.000000000000000000 ) ) ;
#3672 = ORIENTED_EDGE ( 'NONE', *, *, #7646, .T. ) ;
#3673 = SHAPE_REPRESENTATION_RELATIONSHIP ( 'NONE' , 'NONE' ,  #3797, #7073 ) ;
#3674 =( BOUNDED_CURVE ( )  B_SPLINE_CURVE ( 2, ( #2923, #4177, #1513, #5039, #2213, #3613, #4949, #2081, #5740 ),
 .UNSPECIFIED., .F., .T. ) 
 B_SPLINE_CURVE_WITH_KNOTS ( ( 3, 2, 2, 2, 3 ),
 ( 0.7708333333333332593, 0.7777777777777777901, 0.7916666666666666297, 0.8055555555555555802, 0.8125000000000000000 ),
 .UNSPECIFIED. ) 
 CURVE ( )  GEOMETRIC_REPRESENTATION_ITEM ( )  RATIONAL_B_SPLINE_CURVE ( ( 0.9330127018922192983, 0.9330127018922187432, 1.000000000000000000, 0.8660254037844387076, 1.000000000000000000, 0.8660254037844387076, 1.000000000000000000, 0.9330127018922194093, 0.9330127018922194093 ) ) 
 REPRESENTATION_ITEM ( '' )  );
#3675 = MECHANICAL_DESIGN_GEOMETRIC_PRESENTATION_REPRESENTATION (  '', ( #9162 ), #7384 ) ;
#3676 = CARTESIAN_POINT ( 'NONE',  ( -5.250000000000000000, -29.50000000000000000, 0.000000000000000000 ) ) ;
#3677 = ORIENTED_EDGE ( 'NONE', *, *, #4836, .F. ) ;
#3678 = CARTESIAN_POINT ( 'NONE',  ( -3.807688866302469071E-16, -27.64062499965859843, -6.218427825808274356 ) ) ;
#3679 = CARTESIAN_POINT ( 'NONE',  ( -1.224499502706140497, -6.450659073900641971, 3.007514324621436863 ) ) ;
#3680 = ORIENTED_EDGE ( 'NONE', *, *, #3665, .F. ) ;
#3681 = CARTESIAN_POINT ( 'NONE',  ( 5.249999999999999112, -29.27083333333333215, 3.031088913245538308 ) ) ;
#3682 = CARTESIAN_POINT ( 'NONE',  ( -1.975475456537005874E-15, -29.81249999999999645, 5.250000000000000000 ) ) ;
#3683 = CARTESIAN_POINT ( 'NONE',  ( 5.114683531250000748, -27.92187500034139802, 0.000000000000000000 ) ) ;
#3684 = CARTESIAN_POINT ( 'NONE',  ( 5.114683531249999859, -27.40104166700806587, -2.952963913586932776 ) ) ;
#3685 = EDGE_CURVE ( 'NONE', #2122, #4375, #8478, .T. ) ;
#3686 = LINE ( 'NONE', #6464, #4761 ) ;
#3687 = CARTESIAN_POINT ( 'NONE',  ( 3.507514324621465285, -4.349340926099361404, -1.431606283892619125 ) ) ;
#3688 = DIRECTION ( 'NONE',  ( 0.000000000000000000, 0.000000000000000000, 1.000000000000000000 ) ) ;
#3689 = DIRECTION ( 'NONE',  ( 0.000000000000000000, 1.000000000000000000, 0.000000000000000000 ) ) ;
#3690 = CARTESIAN_POINT ( 'NONE',  ( -1.431606283892620235, -6.349340926099360516, -3.507514324621463953 ) ) ;
#3691 = CARTESIAN_POINT ( 'NONE',  ( 5.249999999999997335, -27.30208333401612819, 3.031088913245538308 ) ) ;
#3692 = ADVANCED_FACE ( 'NONE', ( #597 ), #7670, .F. ) ;
#3693 = VERTEX_POINT ( 'NONE', #6780 ) ;
#3694 = CARTESIAN_POINT ( 'NONE',  ( 2.625000000000002220, -27.16666666666666430, 4.546633369868302132 ) ) ;
#3695 = CARTESIAN_POINT ( 'NONE',  ( 1.406733260263394625, -27.94866454968462222, -5.250000000000000000 ) ) ;
#3696 = CARTESIAN_POINT ( 'NONE',  ( -2.557341765624999042, -28.77604166700806587, -4.429445870380400052 ) ) ;
#3697 = VECTOR ( 'NONE', #2221, 1000.000000000000000 ) ;
#3698 = ORIENTED_EDGE ( 'NONE', *, *, #7150, .T. ) ;
#3699 = EDGE_LOOP ( 'NONE', ( #3096, #5860, #4421, #656, #6195, #3921, #6067, #6710 ) ) ;
#3700 = CARTESIAN_POINT ( 'NONE',  ( 6.429395695523604153E-16, -30.00000000000000000, -5.250000000000000000 ) ) ;
#3701 = CARTESIAN_POINT ( 'NONE',  ( 5.385316468750000141, -27.48437499965860198, -6.595110575850215044E-16 ) ) ;
#3702 = CARTESIAN_POINT ( 'NONE',  ( 1.638713065079161924, -0.7493409260993607601, 4.007514324621467949 ) ) ;
#3703 = CARTESIAN_POINT ( 'NONE',  ( 6.972266317189433020E-16, -29.21875000068279249, -5.249999999999999112 ) ) ;
#3704 = MECHANICAL_DESIGN_GEOMETRIC_PRESENTATION_REPRESENTATION (  '', ( #3419 ), #8602 ) ;
#3705 = VERTEX_POINT ( 'NONE', #406 ) ;
#3706 = CARTESIAN_POINT ( 'NONE',  ( 1.975475456537005874E-15, -27.87499999931720041, 5.250000000000000000 ) ) ;
#3707 = CARTESIAN_POINT ( 'NONE',  ( 5.250000000000000000, -29.78125000068279604, 0.000000000000000000 ) ) ;
#3708 = CARTESIAN_POINT ( 'NONE',  ( -2.692658234374996518, -27.56770833299193413, 4.663820869356208654 ) ) ;
#3709 = AXIS2_PLACEMENT_3D ( 'NONE', #7611, #346, #4077 ) ;
#3710 = CARTESIAN_POINT ( 'NONE',  ( -2.557341765624999042, -27.27604166700806587, -4.429445870380400052 ) ) ;
#3711 = CARTESIAN_POINT ( 'NONE',  ( 1.467888652719048226, -1.349340926099361182, -3.492485675378536047 ) ) ;
#3712 = CARTESIAN_POINT ( 'NONE',  ( 5.385316468750000141, -27.20312499965860198, -6.595110575850215044E-16 ) ) ;
#3713 = CARTESIAN_POINT ( 'NONE',  ( 0.01814118441314514080, -4.950659073900641083, 3.000000000000000444 ) ) ;
#3714 = CIRCLE ( 'NONE', #7274, 2.050090691792606279 ) ;
#3715 = CARTESIAN_POINT ( 'NONE',  ( 2.161402558328724325E-14, -29.49999999931720396, -5.250000000000000000 ) ) ;
#3716 = CARTESIAN_POINT ( 'NONE',  ( -4.000000000000000000, -1.849340926099360738, -0.01814118441321865144 ) ) ;
#3717 = AXIS2_PLACEMENT_3D ( 'NONE', #4887, #4762, #1230 ) ;
#3718 = CARTESIAN_POINT ( 'NONE',  ( -2.624999999999996891, -28.14583333265053255, 4.546633369868304797 ) ) ;
#3719 = CARTESIAN_POINT ( 'NONE',  ( 2.624999999999998668, -27.58333333333333570, -4.546633369868303021 ) ) ;
#3720 = CARTESIAN_POINT ( 'NONE',  ( 3.492485675378535603, -4.149340926099362115, 1.467888652719046672 ) ) ;
#3721 = VECTOR ( 'NONE', #2760, 1000.000000000000000 ) ;
#3722 = CARTESIAN_POINT ( 'NONE',  ( 2.625000000000002220, -29.60416666598386826, 4.546633369868302132 ) ) ;
#3723 = EDGE_CURVE ( 'NONE', #2779, #7570, #5575, .T. ) ;
#3724 = ORIENTED_EDGE ( 'NONE', *, *, #1329, .T. ) ;
#3725 = DIRECTION ( 'NONE',  ( 0.000000000000000000, 0.000000000000000000, 1.000000000000000000 ) ) ;
#3726 = CARTESIAN_POINT ( 'NONE',  ( -3.807688866302469071E-16, -28.14062499965860198, -6.218427825808274356 ) ) ;
#3727 = CARTESIAN_POINT ( 'NONE',  ( -2.815599370228846876, -3.249340926099360871, -2.841254879263533262 ) ) ;
#3728 = CARTESIAN_POINT ( 'NONE',  ( 0.000000000000000000, -30.00000000000000000, 0.000000000000000000 ) ) ;
#3729 = ORIENTED_EDGE ( 'NONE', *, *, #7817, .T. ) ;
#3730 = CARTESIAN_POINT ( 'NONE',  ( -1.084901341431563726E-15, -26.92187500034139802, 5.905927827173866440 ) ) ;
#3731 = CARTESIAN_POINT ( 'NONE',  ( -3.492485675378566246, 0.1493409260993610876, 1.467888652718973397 ) ) ;
#3732 = AXIS2_PLACEMENT_3D ( 'NONE', #9184, #7098, #722 ) ;
#3733 = ORIENTED_EDGE ( 'NONE', *, *, #2410, .T. ) ;
#3734 = CARTESIAN_POINT ( 'NONE',  ( -2.625000000000002220, -29.08333333333333215, 4.546633369868302132 ) ) ;
#3735 = APPLICATION_CONTEXT ( 'automotive_design' ) ;
#3736 = CARTESIAN_POINT ( 'NONE',  ( -1.084901341431563726E-15, -27.73437500034139802, 5.905927827173866440 ) ) ;
#3737 = ADVANCED_FACE ( 'NONE', ( #3302 ), #8963, .T. ) ;
#3738 = AXIS2_PLACEMENT_3D ( 'NONE', #4920, #5754, #7769 ) ;
#3739 = CARTESIAN_POINT ( 'NONE',  ( -5.249999999999999112, -29.42708333401613174, -3.031088913245536975 ) ) ;
#3740 = EDGE_CURVE ( 'NONE', #8455, #4014, #3087, .T. ) ;
#3741 = DIRECTION ( 'NONE',  ( 0.000000000000000000, 1.000000000000000000, 0.000000000000000000 ) ) ;
#3742 = CARTESIAN_POINT ( 'NONE',  ( -2.487701488670255312, -6.849340926099361404, 2.462045979635577808 ) ) ;
#3743 = FACE_OUTER_BOUND ( 'NONE', #6302, .T. ) ;
#3744 = CARTESIAN_POINT ( 'NONE',  ( 0.000000000000000000, -30.00000000000000000, -5.242490174541154069 ) ) ;
#3745 = CARTESIAN_POINT ( 'NONE',  ( 1.467888652719048226, -7.749340926099361759, -3.492485675378536047 ) ) ;
#3746 =( NAMED_UNIT ( * ) PLANE_ANGLE_UNIT ( ) SI_UNIT ( $, .RADIAN. ) );
#3747 = ORIENTED_EDGE ( 'NONE', *, *, #4815, .T. ) ;
#3748 = CARTESIAN_POINT ( 'NONE',  ( 5.250000000000000000, -27.03125000068279604, 0.000000000000000000 ) ) ;
#3749 = CARTESIAN_POINT ( 'NONE',  ( -2.557341765624999042, -29.02604166700806587, -4.429445870380400052 ) ) ;
#3750 = ORIENTED_EDGE ( 'NONE', *, *, #609, .F. ) ;
#3751 = DIRECTION ( 'NONE',  ( 1.000000000000000000, 0.000000000000000000, 0.000000000000000000 ) ) ;
#3752 = CARTESIAN_POINT ( 'NONE',  ( -5.385316468749998364, -27.83854166632526628, 3.109213912904140287 ) ) ;
#3753 = CARTESIAN_POINT ( 'NONE',  ( -2.815599370228907272, -6.350659073900638774, 2.841254879263473754 ) ) ;
#3754 = CARTESIAN_POINT ( 'NONE',  ( 1.406733260263405061, -27.44866454968462932, -5.249999999999994671 ) ) ;
#3755 = ORIENTED_EDGE ( 'NONE', *, *, #2044, .T. ) ;
#3756 = CARTESIAN_POINT ( 'NONE',  ( 1.406733260263385521, -29.92633545031537068, 5.250000000000006217 ) ) ;
#3757 = CARTESIAN_POINT ( 'NONE',  ( 3.712013335537174572E-16, -29.21875000068279249, -6.062177826491070398 ) ) ;
#3758 = CARTESIAN_POINT ( 'NONE',  ( 5.385316468750001029, -27.75520833299194123, 3.109213912904135846 ) ) ;
#3759 = CARTESIAN_POINT ( 'NONE',  ( -5.114683531250000748, -29.77604166700806232, 2.952963913586931888 ) ) ;
#3760 = CARTESIAN_POINT ( 'NONE',  ( -0.01814118441321365544, -0.6493409260993610044, 3.500000000000000000 ) ) ;
#3761 = CARTESIAN_POINT ( 'NONE',  ( -2.692658234375000514, -27.36979166632526628, -4.663820869356205989 ) ) ;
#3762 = CARTESIAN_POINT ( 'NONE',  ( 1.260781871532430598, -0.2506590739006394064, 2.992485675378564469 ) ) ;
#3763 = UNCERTAINTY_MEASURE_WITH_UNIT (LENGTH_MEASURE( 1.000000000000000082E-05 ), #145, 'distance_accuracy_value', 'NONE');
#3764 = CARTESIAN_POINT ( 'NONE',  ( -1.406733260263391960, -27.38616454900182973, 5.250000000000000000 ) ) ;
#3765 = CARTESIAN_POINT ( 'NONE',  ( 1.638713065079247855, -7.250659073900640017, -4.007514324621431534 ) ) ;
#3766 = AXIS2_PLACEMENT_3D ( 'NONE', #6927, #1112, #5380 ) ;
#3767 = AXIS2_PLACEMENT_3D ( 'NONE', #5405, #1490, #1441 ) ;
#3768 = CARTESIAN_POINT ( 'NONE',  ( 2.625000000000002220, -27.85416666598386826, 4.546633369868302132 ) ) ;
#3769 = CARTESIAN_POINT ( 'NONE',  ( -5.249999999999999112, -27.70833333265053255, -3.031088913245534755 ) ) ;
#3770 = CARTESIAN_POINT ( 'NONE',  ( 2.462045979635577364, -4.049340926099360694, 2.487701488670255312 ) ) ;
#3771 = DIRECTION ( 'NONE',  ( 0.000000000000000000, 0.000000000000000000, -1.000000000000000000 ) ) ;
#3772 = SURFACE_STYLE_FILL_AREA ( #3077 ) ;
#3773 = CARTESIAN_POINT ( 'NONE',  ( -2.692658234374996518, -27.78645833299193413, 4.663820869356208654 ) ) ;
#3774 = CARTESIAN_POINT ( 'NONE',  ( 1.674995433905601239, -4.549340926099363358, -3.992485675378532939 ) ) ;
#3775 = AXIS2_PLACEMENT_3D ( 'NONE', #8021, #209, #3751 ) ;
#3776 = CARTESIAN_POINT ( 'NONE',  ( 2.161402558328724325E-14, -28.56250000000000000, -5.250000000000000000 ) ) ;
#3777 = ORIENTED_EDGE ( 'NONE', *, *, #9125, .T. ) ;
#3778 = FACE_OUTER_BOUND ( 'NONE', #396, .T. ) ;
#3779 = CARTESIAN_POINT ( 'NONE',  ( 3.500000000000000000, -0.5506590739006389512, -0.01814118441313969030 ) ) ;
#3780 = VERTEX_POINT ( 'NONE', #119 ) ;
#3781 = CARTESIAN_POINT ( 'NONE',  ( 5.249999999999999112, -27.27083333333332860, 3.031088913245538308 ) ) ;
#3782 = VECTOR ( 'NONE', #2492, 1000.000000000000000 ) ;
#3783 = CARTESIAN_POINT ( 'NONE',  ( 5.114683531249998971, -27.69270833367473017, 2.952963913586936329 ) ) ;
#3784 = ADVANCED_FACE ( 'NONE', ( #6485 ), #7849, .F. ) ;
#3785 = CARTESIAN_POINT ( 'NONE',  ( -1.084901341431563923E-15, -26.98437500034139802, 5.905927827173866440 ) ) ;
#3786 = DIRECTION ( 'NONE',  ( 0.000000000000000000, 1.000000000000000000, 0.000000000000000000 ) ) ;
#3787 = EDGE_CURVE ( 'NONE', #8000, #7866, #75, .T. ) ;
#3788 = CARTESIAN_POINT ( 'NONE',  ( -1.431606283892620235, -4.749340926099363536, -3.507514324621463953 ) ) ;
#3789 = CARTESIAN_POINT ( 'NONE',  ( -2.033577675846918216E-14, -29.87499999931720396, 5.250000000000000888 ) ) ;
#3790 = LINE ( 'NONE', #8615, #6417 ) ;
#3791 = CARTESIAN_POINT ( 'NONE',  ( -5.114683531249999859, -28.31770833367473372, -2.952963913586935440 ) ) ;
#3792 = DIRECTION ( 'NONE',  ( 0.000000000000000000, 0.000000000000000000, -1.000000000000000000 ) ) ;
#3793 = VERTEX_POINT ( 'NONE', #7758 ) ;
#3794 = CARTESIAN_POINT ( 'NONE',  ( 0.000000000000000000, 73.00000000000001421, -3.000000000000000444 ) ) ;
#3795 = CARTESIAN_POINT ( 'NONE',  ( 5.114683531250000748, -28.60937500034139802, 0.000000000000000000 ) ) ;
#3796 = ADVANCED_FACE ( 'NONE', ( #7193 ), #4992, .T. ) ;
#3797 = SHAPE_REPRESENTATION ( 'top sleeve', ( #888 ), #6054 ) ;
#3798 = EDGE_LOOP ( 'NONE', ( #8560, #7747 ) ) ;
#3799 = CARTESIAN_POINT ( 'NONE',  ( -2.625000000000000444, -29.79166666666666785, -4.546633369868303021 ) ) ;
#3800 = CARTESIAN_POINT ( 'NONE',  ( 2.692658234375002735, -27.52604166632526628, 4.663820869356205101 ) ) ;
#3801 = CARTESIAN_POINT ( 'NONE',  ( 1.638713065079247855, -5.650659073900638596, -4.007514324621431534 ) ) ;
#3802 = VERTEX_POINT ( 'NONE', #2969 ) ;
#3803 = FACE_OUTER_BOUND ( 'NONE', #7304, .T. ) ;
#3804 = CARTESIAN_POINT ( 'NONE',  ( 5.385316468749999252, -27.96354166632526628, -3.109213912904139399 ) ) ;
#3805 = CARTESIAN_POINT ( 'NONE',  ( 5.114683531249998971, -27.88020833367473017, 2.952963913586936329 ) ) ;
#3806 = EDGE_LOOP ( 'NONE', ( #2960, #7095 ) ) ;
#3807 = DIRECTION ( 'NONE',  ( 0.000000000000000000, 0.000000000000000000, 1.000000000000000000 ) ) ;
#3808 = CARTESIAN_POINT ( 'NONE',  ( -1.260781871532431708, -2.650659073900639928, -2.992485675378564469 ) ) ;
#3809 = DIRECTION ( 'NONE',  ( 0.8660254037844402619, -0.4999999999999970579, 0.000000000000000000 ) ) ;
#3810 = ADVANCED_FACE ( 'NONE', ( #5611 ), #8458, .F. ) ;
#3811 = CARTESIAN_POINT ( 'NONE',  ( 1.113604000661152470E-15, -27.62499999931720396, 6.062177826491070398 ) ) ;
#3812 = CARTESIAN_POINT ( 'NONE',  ( 3.367778697655221012E-16, -9.999999999999998224, -2.750000000000000000 ) ) ;
#3813 = CARTESIAN_POINT ( 'NONE',  ( -3.492485675378535603, -4.949340926099361049, -1.467888652719048670 ) ) ;
#3814 = DIRECTION ( 'NONE',  ( 0.000000000000000000, 0.000000000000000000, -1.000000000000000000 ) ) ;
#3815 = ORIENTED_EDGE ( 'NONE', *, *, #2428, .T. ) ;
#3816 = CARTESIAN_POINT ( 'NONE',  ( 0.000000000000000000, 0.000000000000000000, 0.000000000000000000 ) ) ;
#3817 = CARTESIAN_POINT ( 'NONE',  ( 1.142306659890740623E-15, -28.26562499965860198, 6.218427825808274356 ) ) ;
#3818 = CARTESIAN_POINT ( 'NONE',  ( 0.01814118441321938349, -4.649340926099361226, -4.000000000000000000 ) ) ;
#3819 = LINE ( 'NONE', #3260, #6360 ) ;
#3820 = ORIENTED_EDGE ( 'NONE', *, *, #2854, .T. ) ;
#3821 = CARTESIAN_POINT ( 'NONE',  ( 2.692658234374998738, -27.91145833299193413, -4.663820869356206877 ) ) ;
#3822 = CARTESIAN_POINT ( 'NONE',  ( -1.467888652718973619, -1.050659073900638951, -3.492485675378565801 ) ) ;
#3823 = ORIENTED_EDGE ( 'NONE', *, *, #8661, .T. ) ;
#3824 = CARTESIAN_POINT ( 'NONE',  ( 5.249999999999999112, -28.02083333333333215, 3.031088913245538308 ) ) ;
#3825 = CARTESIAN_POINT ( 'NONE',  ( -3.500000000000000000, -2.950659073900639306, 0.01814118441314012051 ) ) ;
#3826 = STYLED_ITEM ( 'NONE', ( #7037 ), #542 ) ;
#3827 = CARTESIAN_POINT ( 'NONE',  ( -3.712013335537174572E-16, -27.31250000000000000, -6.062177826491070398 ) ) ;
#3828 = CARTESIAN_POINT ( 'NONE',  ( 5.114683531250000748, -29.33854166700806232, -2.952963913586932776 ) ) ;
#3829 = CARTESIAN_POINT ( 'NONE',  ( 2.487701488670255756, -1.249340926099361093, -2.462045979635577364 ) ) ;
#3830 = LINE ( 'NONE', #2387, #2829 ) ;
#3831 = CARTESIAN_POINT ( 'NONE',  ( 2.300847884672513123E-14, -27.46875000068279604, -5.250000000000000000 ) ) ;
#3832 = CARTESIAN_POINT ( 'NONE',  ( -1.084901341431563923E-15, -29.23437500034139802, 5.905927827173866440 ) ) ;
#3833 =( GEOMETRIC_REPRESENTATION_CONTEXT ( 3 ) GLOBAL_UNCERTAINTY_ASSIGNED_CONTEXT ( ( #3660 ) ) GLOBAL_UNIT_ASSIGNED_CONTEXT ( ( #4661, #8978, #5492 ) ) REPRESENTATION_CONTEXT ( 'NONE', 'WORKASPACE' ) );
#3834 = ORIENTED_EDGE ( 'NONE', *, *, #1174, .T. ) ;
#3835 = CARTESIAN_POINT ( 'NONE',  ( 6.972266317189433020E-16, -26.96875000068279249, -5.250000000000000000 ) ) ;
#3836 = CARTESIAN_POINT ( 'NONE',  ( -2.557341765625002594, -28.19270833367473017, 4.429445870380399164 ) ) ;
#3837 = AXIS2_PLACEMENT_3D ( 'NONE', #5152, #5991, #5247 ) ;
#3838 = ORIENTED_EDGE ( 'NONE', *, *, #5661, .F. ) ;
#3839 = EDGE_CURVE ( 'NONE', #8840, #301, #1467, .T. ) ;
#3840 = CARTESIAN_POINT ( 'NONE',  ( 2.161402558328724325E-14, -29.56250000000000355, -5.250000000000000000 ) ) ;
#3841 = CARTESIAN_POINT ( 'NONE',  ( 5.204748896376250699E-16, -30.00000000000000000, -4.250000000000000000 ) ) ;
#3842 = CARTESIAN_POINT ( 'NONE',  ( 4.000000000000000000, -5.350659073900637885, -0.01814118441313441674 ) ) ;
#3843 = FILL_AREA_STYLE ('',( #6528 ) ) ;
#3844 = CARTESIAN_POINT ( 'NONE',  ( -5.385316468750000141, -28.35937499965860198, 0.000000000000000000 ) ) ;
#3845 = ORIENTED_EDGE ( 'NONE', *, *, #6275, .T. ) ;
#3846 =( BOUNDED_CURVE ( )  B_SPLINE_CURVE ( 2, ( #2348, #5178, #853, #8581, #8069 ),
 .UNSPECIFIED., .F., .F. ) 
 B_SPLINE_CURVE_WITH_KNOTS ( ( 3, 2, 3 ),
 ( 0.9791666666666667407, 0.9861111111111111605, 1.000000000000000000 ),
 .UNSPECIFIED. ) 
 CURVE ( )  GEOMETRIC_REPRESENTATION_ITEM ( )  RATIONAL_B_SPLINE_CURVE ( ( 0.9330127018922192983, 0.9330127018922198534, 1.000000000000000000, 0.8660254037844387076, 1.000000000000000000 ) ) 
 REPRESENTATION_ITEM ( '' )  );
#3847 = DIRECTION ( 'NONE',  ( -0.000000000000000000, -1.000000000000000000, -0.000000000000000000 ) ) ;
#3848 = CARTESIAN_POINT ( 'NONE',  ( -2.624999999999998668, -29.69791666734946034, -4.546633369868303021 ) ) ;
#3849 = CARTESIAN_POINT ( 'NONE',  ( -5.385316468750001029, -28.38020833299193058, -3.109213912904136734 ) ) ;
#3850 = ADVANCED_FACE ( 'NONE', ( #2215 ), #9060, .T. ) ;
#3851 = CARTESIAN_POINT ( 'NONE',  ( -5.114683531249999859, -29.56770833367473017, -2.952963913586935440 ) ) ;
#3852 = EDGE_LOOP ( 'NONE', ( #7270, #6818, #5417, #3946 ) ) ;
#3853 = VECTOR ( 'NONE', #1936, 1000.000000000000000 ) ;
#3854 =( REPRESENTATION_RELATIONSHIP ('NONE','NONE', #735, #4551 ) REPRESENTATION_RELATIONSHIP_WITH_TRANSFORMATION ( #7584 )SHAPE_REPRESENTATION_RELATIONSHIP( ) );
#3855 = CARTESIAN_POINT ( 'NONE',  ( 2.161402558328724325E-14, -28.74999999931720751, -5.250000000000000000 ) ) ;
#3856 = CARTESIAN_POINT ( 'NONE',  ( 1.260781871532430598, -1.850659073900639884, 2.992485675378564469 ) ) ;
#3857 = CYLINDRICAL_SURFACE ( 'NONE', #7714, 5.250000000000000000 ) ;
#3858 = CARTESIAN_POINT ( 'NONE',  ( -2.625000000000000444, -28.22916666598386826, -4.546633369868303021 ) ) ;
#3859 = CARTESIAN_POINT ( 'NONE',  ( 0.000000000000000000, -35.00000000000000000, 0.000000000000000000 ) ) ;
#3860 = CARTESIAN_POINT ( 'NONE',  ( 3.507514324621465285, -2.749340926099361315, -1.431606283892619347 ) ) ;
#3861 = EDGE_CURVE ( 'NONE', #3693, #566, #5272, .T. ) ;
#3862 = CARTESIAN_POINT ( 'NONE',  ( 0.000000000000000000, 75.00000000000000000, 4.250000000000000000 ) ) ;
#3863 = DIRECTION ( 'NONE',  ( 0.000000000000000000, 0.000000000000000000, 1.000000000000000000 ) ) ;
#3864 = CARTESIAN_POINT ( 'NONE',  ( -5.385316468750000141, -28.57812499965860198, 0.000000000000000000 ) ) ;
#3865 = CARTESIAN_POINT ( 'NONE',  ( 2.815599370228847320, -5.649340926099361226, 2.841254879263533262 ) ) ;
#3866 = CARTESIAN_POINT ( 'NONE',  ( 1.000000000000000000, -35.00000000000000000, -2.880243826144208708 ) ) ;
#3867 = ORIENTED_EDGE ( 'NONE', *, *, #814, .F. ) ;
#3868 = CIRCLE ( 'NONE', #5934, 4.000000000000000000 ) ;
#3869 = CLOSED_SHELL ( 'NONE', ( #1199, #7781, #4657, #2768, #5305, #6558, #2850, #1975, #3784 ) ) ;
#3870 = CARTESIAN_POINT ( 'NONE',  ( 5.385316468750000141, -27.95312499965860198, -6.595110575850215044E-16 ) ) ;
#3871 = CARTESIAN_POINT ( 'NONE',  ( -0.01814118441313947866, -5.750659073900639129, -3.500000000000000000 ) ) ;
#3872 = VERTEX_POINT ( 'NONE', #8544 ) ;
#3873 = CARTESIAN_POINT ( 'NONE',  ( 2.624999999999996891, -27.54166666666666430, 4.546633369868304797 ) ) ;
#3874 = AXIS2_PLACEMENT_3D ( 'NONE', #2925, #723, #5792 ) ;
#3875 = CARTESIAN_POINT ( 'NONE',  ( -0.01814118441313947866, -0.9506590739006390844, -3.500000000000000000 ) ) ;
#3876 = EDGE_LOOP ( 'NONE', ( #6690, #4126, #7029, #3268 ) ) ;
#3877 = CARTESIAN_POINT ( 'NONE',  ( -2.625000000000000444, -27.54166666666666430, -4.546633369868303021 ) ) ;
#3878 = CIRCLE ( 'NONE', #899, 3.000000000000000444 ) ;
#3879 = VERTEX_POINT ( 'NONE', #3483 ) ;
#3880 = CARTESIAN_POINT ( 'NONE',  ( -2.557341765625002594, -29.44270833367473017, 4.429445870380399164 ) ) ;
#3881 = CARTESIAN_POINT ( 'NONE',  ( -1.467888652719046449, -5.349340926099361404, 3.492485675378536047 ) ) ;
#3882 = DIRECTION ( 'NONE',  ( -0.000000000000000000, -1.000000000000000000, -0.000000000000000000 ) ) ;
#3883 = DIRECTION ( 'NONE',  ( 0.000000000000000000, 0.000000000000000000, 1.000000000000000000 ) ) ;
#3884 = CARTESIAN_POINT ( 'NONE',  ( 5.114683531249999859, -28.90104166700806942, -2.952963913586932776 ) ) ;
#3885 =( NAMED_UNIT ( * ) SI_UNIT ( $, .STERADIAN. ) SOLID_ANGLE_UNIT ( ) );
#3886 = ADVANCED_FACE ( 'NONE', ( #3527 ), #166, .T. ) ;
#3887 = CARTESIAN_POINT ( 'NONE',  ( 1.406733260263400176, -29.19866454968462932, -5.249999999999997335 ) ) ;
#3888 =( GEOMETRIC_REPRESENTATION_CONTEXT ( 3 ) GLOBAL_UNCERTAINTY_ASSIGNED_CONTEXT ( ( #4539 ) ) GLOBAL_UNIT_ASSIGNED_CONTEXT ( ( #4046, #2652, #5427 ) ) REPRESENTATION_CONTEXT ( 'NONE', 'WORKASPACE' ) );
#3889 = CARTESIAN_POINT ( 'NONE',  ( -2.557341765625002594, -27.69270833367473017, 4.429445870380399164 ) ) ;
#3890 = VERTEX_POINT ( 'NONE', #2998 ) ;
#3891 = CARTESIAN_POINT ( 'NONE',  ( 1.406733260263398400, -27.82366454968462932, -5.249999999999997335 ) ) ;
#3892 = CARTESIAN_POINT ( 'NONE',  ( 5.385316468750000141, -28.73437499965860198, -6.595110575850215044E-16 ) ) ;
#3893 = CARTESIAN_POINT ( 'NONE',  ( 4.007514324621469726, -1.149340926099360782, -1.638713065079161257 ) ) ;
#3894 = DIRECTION ( 'NONE',  ( 0.000000000000000000, 0.000000000000000000, 1.000000000000000000 ) ) ;
#3895 = CARTESIAN_POINT ( 'NONE',  ( -5.385316468750001029, -29.63020833299193768, -3.109213912904136734 ) ) ;
#3896 = ORIENTED_EDGE ( 'NONE', *, *, #1249, .F. ) ;
#3897 = DIRECTION ( 'NONE',  ( -0.000000000000000000, -1.000000000000000000, -0.000000000000000000 ) ) ;
#3898 = CARTESIAN_POINT ( 'NONE',  ( -5.250000000000000888, -28.63541666734946389, 3.031088913245532979 ) ) ;
#3899 = CARTESIAN_POINT ( 'NONE',  ( -2.692658234374996518, -27.31770833299193413, 4.663820869356208654 ) ) ;
#3900 = ORIENTED_EDGE ( 'NONE', *, *, #1184, .T. ) ;
#3901 = CARTESIAN_POINT ( 'NONE',  ( -2.692658234375000514, -27.86979166632526628, -4.663820869356205989 ) ) ;
#3902 = CARTESIAN_POINT ( 'NONE',  ( 3.000000000000000444, -2.150659073900639484, -0.01814118441314496039 ) ) ;
#3903 = CARTESIAN_POINT ( 'NONE',  ( 3.673940397442060361E-16, 70.00000000000000000, 3.000000000000000444 ) ) ;
#3904 =( BOUNDED_CURVE ( )  B_SPLINE_CURVE ( 2, ( #6877, #9005, #505, #3348, #5473 ),
 .UNSPECIFIED., .F., .F. ) 
 B_SPLINE_CURVE_WITH_KNOTS ( ( 3, 2, 3 ),
 ( 0.000000000000000000, 0.01388888888888888812, 0.02083333333333333218 ),
 .UNSPECIFIED. ) 
 CURVE ( )  GEOMETRIC_REPRESENTATION_ITEM ( )  RATIONAL_B_SPLINE_CURVE ( ( 1.000000000000000000, 0.8660254037844387076, 1.000000000000000000, 0.9330127018922194093, 0.9330127018922194093 ) ) 
 REPRESENTATION_ITEM ( '' )  );
#3905 = CARTESIAN_POINT ( 'NONE',  ( 5.250000000000000000, -27.79166666598386826, -3.031088913245536531 ) ) ;
#3906 = FACE_OUTER_BOUND ( 'NONE', #19, .T. ) ;
#3907 = CARTESIAN_POINT ( 'NONE',  ( 2.462045979635577364, -5.649340926099361226, 2.487701488670255312 ) ) ;
#3908 = EDGE_CURVE ( 'NONE', #4607, #5775, #4385, .T. ) ;
#3909 = CARTESIAN_POINT ( 'NONE',  ( -2.557341765624999042, -29.52604166700806232, -4.429445870380400052 ) ) ;
#3910 = CARTESIAN_POINT ( 'NONE',  ( -3.807688866302469071E-16, -29.89062499965859843, -6.218427825808274356 ) ) ;
#3911 = CARTESIAN_POINT ( 'NONE',  ( -3.992485675378532939, -3.349340926099360960, -1.674995433905601683 ) ) ;
#3912 = CARTESIAN_POINT ( 'NONE',  ( -1.406733260263384411, -28.55133545031537068, -5.250000000000006217 ) ) ;
#3913 = AXIS2_PLACEMENT_3D ( 'NONE', #640, #3485, #8326 ) ;
#3914 = ORIENTED_EDGE ( 'NONE', *, *, #1403, .F. ) ;
#3915 = CARTESIAN_POINT ( 'NONE',  ( -5.385316468750001029, -27.84895833299193413, -3.109213912904136734 ) ) ;
#3916 = CARTESIAN_POINT ( 'NONE',  ( 3.492485675378566690, -5.450659073900639306, -1.467888652718972287 ) ) ;
#3917 = EDGE_LOOP ( 'NONE', ( #6738, #2442, #7210, #5313 ) ) ;
#3918 = CARTESIAN_POINT ( 'NONE',  ( -5.250000000000000000, -27.64583333333333215, -3.031088913245536531 ) ) ;
#3919 = CARTESIAN_POINT ( 'NONE',  ( 5.250000000000000000, -27.12500000000000000, -6.429395695523604153E-16 ) ) ;
#3920 = CARTESIAN_POINT ( 'NONE',  ( 3.492485675378566690, -2.250659073900639573, -1.467888652718972287 ) ) ;
#3921 = ORIENTED_EDGE ( 'NONE', *, *, #7992, .F. ) ;
#3922 =( LENGTH_UNIT ( ) NAMED_UNIT ( * ) SI_UNIT ( .MILLI., .METRE. ) );
#3923 = CARTESIAN_POINT ( 'NONE',  ( -2.624999999999998668, -29.44791666734946034, -4.546633369868303021 ) ) ;
#3924 = ORIENTED_EDGE ( 'NONE', *, *, #4012, .F. ) ;
#3925 = CARTESIAN_POINT ( 'NONE',  ( -5.114683531250000748, -28.75520833367473017, -2.952963913586935440 ) ) ;
#3926 = CARTESIAN_POINT ( 'NONE',  ( 2.134148098076978251, -1.249340926099361537, -2.108492589042307408 ) ) ;
#3927 = FACE_OUTER_BOUND ( 'NONE', #6004, .T. ) ;
#3928 = CARTESIAN_POINT ( 'NONE',  ( -1.000000000000000000, -29.00000000000000355, -2.431755684948965435 ) ) ;
#3929 = CARTESIAN_POINT ( 'NONE',  ( 2.557341765624996821, -28.96354166700806587, 4.429445870380401828 ) ) ;
#3930 = DIRECTION ( 'NONE',  ( 0.000000000000000000, -1.000000000000000000, 0.000000000000000000 ) ) ;
#3931 = CIRCLE ( 'NONE', #3775, 2.500000000000000444 ) ;
#3932 = CARTESIAN_POINT ( 'NONE',  ( -1.953518037137212504, -4.474939649319626956E-16, 2.844108989334067861 ) ) ;
#3933 = CARTESIAN_POINT ( 'NONE',  ( -2.557341765624999042, -27.52604166700806587, -4.429445870380400052 ) ) ;
#3934 = ORIENTED_EDGE ( 'NONE', *, *, #1538, .F. ) ;
#3935 = CARTESIAN_POINT ( 'NONE',  ( 0.000000000000000000, 73.00000000000001421, -3.000000000000000444 ) ) ;
#3936 = CARTESIAN_POINT ( 'NONE',  ( 5.385316468750001029, -29.25520833299193058, 3.109213912904134958 ) ) ;
#3937 = CARTESIAN_POINT ( 'NONE',  ( -3.807688866302469071E-16, -29.92187499965859843, -6.218427825808274356 ) ) ;
#3938 = DIRECTION ( 'NONE',  ( 0.000000000000000000, 1.000000000000000000, 0.000000000000000000 ) ) ;
#3939 = CARTESIAN_POINT ( 'NONE',  ( -2.692658234374996518, -29.81770833299193413, 4.663820869356208654 ) ) ;
#3940 = CARTESIAN_POINT ( 'NONE',  ( 3.992485675378533383, -4.149340926099362115, 1.674995433905599462 ) ) ;
#3941 = ORIENTED_EDGE ( 'NONE', *, *, #7926, .F. ) ;
#3942 = PRODUCT_DEFINITION ( 'UNKNOWN', '', #9030, #6845 ) ;
#3943 = CARTESIAN_POINT ( 'NONE',  ( -5.250000000000000000, -27.42708333401613174, -3.031088913245536531 ) ) ;
#3944 = CARTESIAN_POINT ( 'NONE',  ( 2.692658234374998738, -29.69270833299193413, -4.663820869356206877 ) ) ;
#3945 = PRODUCT_DEFINITION_CONTEXT ( 'detailed design', #2427, 'design' ) ;
#3946 = ORIENTED_EDGE ( 'NONE', *, *, #867, .F. ) ;
#3947 = CARTESIAN_POINT ( 'NONE',  ( 5.385316468749999252, -28.68229166632526983, -3.109213912904138954 ) ) ;
#3948 = CARTESIAN_POINT ( 'NONE',  ( 1.260781871532430598, -6.650659073900641260, 2.992485675378564469 ) ) ;
#3949 = DIRECTION ( 'NONE',  ( 0.000000000000000000, 1.000000000000000000, 0.000000000000000000 ) ) ;
#3950 = EDGE_CURVE ( 'NONE', #3429, #2713, #3686, .T. ) ;
#3951 = CARTESIAN_POINT ( 'NONE',  ( -5.250000000000000000, -28.87499999999999645, -6.429395695523604153E-16 ) ) ;
#3952 = CARTESIAN_POINT ( 'NONE',  ( 6.429395695523604153E-16, -30.00000000000000000, -5.250000000000000000 ) ) ;
#3953 = CARTESIAN_POINT ( 'NONE',  ( -1.431606283892620235, -6.349340926099361404, -3.507514324621463953 ) ) ;
#3954 = CARTESIAN_POINT ( 'NONE',  ( 5.114683531250000748, -29.85937500034139802, 0.000000000000000000 ) ) ;
#3955 = CARTESIAN_POINT ( 'NONE',  ( 2.300847884672513123E-14, -27.68750000000000000, -5.250000000000000000 ) ) ;
#3956 = APPLICATION_PROTOCOL_DEFINITION ( 'draft international standard', 'automotive_design', 1998, #7965 ) ;
#3957 = CARTESIAN_POINT ( 'NONE',  ( 5.385316468750001029, -29.97395833299194123, 3.109213912904135846 ) ) ;
#3958 = CARTESIAN_POINT ( 'NONE',  ( -3.492485675378536047, -3.349340926099361404, -1.467888652719048670 ) ) ;
#3959 = EDGE_CURVE ( 'NONE', #2168, #8645, #5723, .T. ) ;
#3960 = CARTESIAN_POINT ( 'NONE',  ( 1.406733260263393293, -28.51116454900183328, -5.250000000000000000 ) ) ;
#3961 = CARTESIAN_POINT ( 'NONE',  ( -2.692658234375000514, -28.61979166632526628, -4.663820869356205989 ) ) ;
#3962 = CARTESIAN_POINT ( 'NONE',  ( 2.487701488670203354, -5.150659073900639484, 2.462045979635629323 ) ) ;
#3963 = VERTEX_POINT ( 'NONE', #98 ) ;
#3964 = CARTESIAN_POINT ( 'NONE',  ( 1.113604000661152470E-15, -30.12499999931720041, 6.062177826491070398 ) ) ;
#3965 = DIRECTION ( 'NONE',  ( 0.000000000000000000, -1.000000000000000000, 0.000000000000000000 ) ) ;
#3966 = CARTESIAN_POINT ( 'NONE',  ( 2.557341765625000818, -27.13020833367473017, -4.429445870380400052 ) ) ;
#3967 = ORIENTED_EDGE ( 'NONE', *, *, #4861, .F. ) ;
#3968 = FILL_AREA_STYLE_COLOUR ( '', #3094 ) ;
#3969 = CARTESIAN_POINT ( 'NONE',  ( -3.712013335537174572E-16, -28.81249999999999645, -6.062177826491070398 ) ) ;
#3970 = ORIENTED_EDGE ( 'NONE', *, *, #7418, .F. ) ;
#3971 = CARTESIAN_POINT ( 'NONE',  ( -5.114683531250001636, -28.71354166700806587, 2.952963913586931444 ) ) ;
#3972 = CARTESIAN_POINT ( 'NONE',  ( -2.992485675378538268, -3.349340926099362292, -1.260781871532495879 ) ) ;
#3973 = CARTESIAN_POINT ( 'NONE',  ( 5.250000000000000000, -28.53125000068279604, 0.000000000000000000 ) ) ;
#3974 = CARTESIAN_POINT ( 'NONE',  ( 3.061616997868382648E-16, 75.00000000000000000, 2.499999999999999556 ) ) ;
#3975 = CARTESIAN_POINT ( 'NONE',  ( 2.557341765625000818, -29.13020833367473017, -4.429445870380400052 ) ) ;
#3976 = CARTESIAN_POINT ( 'NONE',  ( -2.033577675846918216E-14, -29.12499999931720751, 5.250000000000000888 ) ) ;
#3977 = DIRECTION ( 'NONE',  ( 0.000000000000000000, 0.000000000000000000, -1.000000000000000000 ) ) ;
#3978 = CARTESIAN_POINT ( 'NONE',  ( 2.557341765624996821, -27.40104166700806587, 4.429445870380401828 ) ) ;
#3979 = VERTEX_POINT ( 'NONE', #8008 ) ;
#3980 =( BOUNDED_CURVE ( )  B_SPLINE_CURVE ( 2, ( #815, #1051, #1195, #1898, #7616, #6820, #497, #8313, #8997 ),
 .UNSPECIFIED., .F., .T. ) 
 B_SPLINE_CURVE_WITH_KNOTS ( ( 3, 2, 2, 2, 3 ),
 ( 0.1458333333333333426, 0.1527777777777777901, 0.1666666666666666574, 0.1805555555555555525, 0.1875000000000000000 ),
 .UNSPECIFIED. ) 
 CURVE ( )  GEOMETRIC_REPRESENTATION_ITEM ( )  RATIONAL_B_SPLINE_CURVE ( ( 0.9330127018922194093, 0.9330127018922194093, 1.000000000000000000, 0.8660254037844387076, 1.000000000000000000, 0.8660254037844387076, 1.000000000000000000, 0.9330127018922194093, 0.9330127018922194093 ) ) 
 REPRESENTATION_ITEM ( '' )  );
#3981 =( GEOMETRIC_REPRESENTATION_CONTEXT ( 3 ) GLOBAL_UNCERTAINTY_ASSIGNED_CONTEXT ( ( #8685 ) ) GLOBAL_UNIT_ASSIGNED_CONTEXT ( ( #1080, #1684, #7454 ) ) REPRESENTATION_CONTEXT ( 'NONE', 'WORKASPACE' ) );
#3982 = DIRECTION ( 'NONE',  ( 0.000000000000000000, 0.000000000000000000, 1.000000000000000000 ) ) ;
#3983 = CARTESIAN_POINT ( 'NONE',  ( 5.385316468749999252, -29.46354166632526983, -3.109213912904138954 ) ) ;
#3984 = EDGE_CURVE ( 'NONE', #2164, #3205, #7138, .T. ) ;
#3985 = DIRECTION ( 'NONE',  ( 0.000000000000000000, -1.000000000000000000, 0.000000000000000000 ) ) ;
#3986 = DIRECTION ( 'NONE',  ( -0.000000000000000000, 1.000000000000000000, -0.000000000000000000 ) ) ;
#3987 = CARTESIAN_POINT ( 'NONE',  ( 2.692658234375002735, -29.52604166632526983, 4.663820869356205101 ) ) ;
#3988 = CARTESIAN_POINT ( 'NONE',  ( 3.492485675378536047, -0.9493409260993610488, 1.467888652719046672 ) ) ;
#3989 = ORIENTED_EDGE ( 'NONE', *, *, #9010, .F. ) ;
#3990 = CARTESIAN_POINT ( 'NONE',  ( -5.249999999999999112, -27.52083333333333570, -3.031088913245534755 ) ) ;
#3991 = CARTESIAN_POINT ( 'NONE',  ( -5.250000000000000888, -28.38541666734946034, 3.031088913245532979 ) ) ;
#3992 = CARTESIAN_POINT ( 'NONE',  ( 5.385316468749999252, -29.46354166632526983, -3.109213912904139399 ) ) ;
#3993 = ORIENTED_EDGE ( 'NONE', *, *, #4097, .F. ) ;
#3994 = CARTESIAN_POINT ( 'NONE',  ( -3.807688866302469071E-16, -28.89062499965860198, -6.218427825808274356 ) ) ;
#3995 = CARTESIAN_POINT ( 'NONE',  ( -0.01814118441314477650, -5.750659073900639129, -3.000000000000000444 ) ) ;
#3996 = LINE ( 'NONE', #2504, #3558 ) ;
#3997 =( LENGTH_UNIT ( ) NAMED_UNIT ( * ) SI_UNIT ( .MILLI., .METRE. ) );
#3998 = CARTESIAN_POINT ( 'NONE',  ( 0.000000000000000000, -9.999999999999998224, 5.750000000000000000 ) ) ;
#3999 = CARTESIAN_POINT ( 'NONE',  ( 5.250000000000000000, -27.37500000000000000, -6.429395695523604153E-16 ) ) ;
#4000 = VECTOR ( 'NONE', #5364, 1000.000000000000000 ) ;
#4001 = LINE ( 'NONE', #8138, #651 ) ;
#4002 = FACE_OUTER_BOUND ( 'NONE', #4221, .T. ) ;
#4003 = APPLICATION_PROTOCOL_DEFINITION ( 'draft international standard', 'automotive_design', 1998, #4323 ) ;
#4004 = CARTESIAN_POINT ( 'NONE',  ( 5.385316468750000141, -29.70312499965859843, -6.595110575850215044E-16 ) ) ;
#4005 = CARTESIAN_POINT ( 'NONE',  ( -0.01814118441321365544, -5.449340926099361937, 3.500000000000000000 ) ) ;
#4006 = CARTESIAN_POINT ( 'NONE',  ( 2.625000000000002220, -28.60416666598386826, 4.546633369868302132 ) ) ;
#4007 = CARTESIAN_POINT ( 'NONE',  ( 5.385316468750000141, -28.45312499965860198, -6.595110575850215044E-16 ) ) ;
#4008 = CARTESIAN_POINT ( 'NONE',  ( 2.462045979635629767, -7.150659073900639484, -2.487701488670203354 ) ) ;
#4009 = VERTEX_POINT ( 'NONE', #7875 ) ;
#4010 = CARTESIAN_POINT ( 'NONE',  ( 5.249999999999999112, -30.04166666598387181, -3.031088913245536975 ) ) ;
#4011 = CARTESIAN_POINT ( 'NONE',  ( 0.000000000000000000, -28.00000000000000000, 0.000000000000000000 ) ) ;
#4012 = EDGE_CURVE ( 'NONE', #2074, #7471, #6987, .T. ) ;
#4013 = CARTESIAN_POINT ( 'NONE',  ( -3.507514324621433754, -1.250659073900639129, -1.431606283892695064 ) ) ;
#4014 = VERTEX_POINT ( 'NONE', #8705 ) ;
#4015 = AXIS2_PLACEMENT_3D ( 'NONE', #6613, #241, #7360 ) ;
#4016 = CARTESIAN_POINT ( 'NONE',  ( -5.249999999999999112, -28.47916666666666785, 3.031088913245538308 ) ) ;
#4017 = ORIENTED_EDGE ( 'NONE', *, *, #4628, .F. ) ;
#4018 = CARTESIAN_POINT ( 'NONE',  ( 5.114683531250000748, -29.35937500034139802, 0.000000000000000000 ) ) ;
#4019 = CARTESIAN_POINT ( 'NONE',  ( -2.134148098076978251, -3.649340926099361671, 2.108492589042307408 ) ) ;
#4020 = DIRECTION ( 'NONE',  ( 0.000000000000000000, 1.000000000000000000, 0.000000000000000000 ) ) ;
#4021 = CARTESIAN_POINT ( 'NONE',  ( -2.557341765624999042, -27.08854166700806232, -4.429445870380400052 ) ) ;
#4022 =( LENGTH_UNIT ( ) NAMED_UNIT ( * ) SI_UNIT ( .MILLI., .METRE. ) );
#4023 = EDGE_CURVE ( 'NONE', #6825, #6014, #2228, .T. ) ;
#4024 = CARTESIAN_POINT ( 'NONE',  ( -2.122541484417015401, -1.321938709600337619E-17, 2.648722836990621499 ) ) ;
#4025 = CARTESIAN_POINT ( 'NONE',  ( 2.557341765625000818, -27.06770833367473017, -4.429445870380400052 ) ) ;
#4026 = CARTESIAN_POINT ( 'NONE',  ( 0.000000000000000000, 0.000000000000000000, 0.000000000000000000 ) ) ;
#4027 = EDGE_CURVE ( 'NONE', #5643, #8929, #8512, .T. ) ;
#4028 = CARTESIAN_POINT ( 'NONE',  ( 2.557341765624996821, -29.46354166700806232, 4.429445870380401828 ) ) ;
#4029 = CARTESIAN_POINT ( 'NONE',  ( 5.250000000000000000, -27.87500000000000000, -6.429395695523604153E-16 ) ) ;
#4030 = CARTESIAN_POINT ( 'NONE',  ( 2.692658234374998738, -28.69270833299193413, -4.663820869356206877 ) ) ;
#4031 = FACE_OUTER_BOUND ( 'NONE', #6432, .T. ) ;
#4032 = DIRECTION ( 'NONE',  ( -1.044949058366720058E-14, -0.07256473765270715637, 0.9973637043974449279 ) ) ;
#4033 = CARTESIAN_POINT ( 'NONE',  ( 5.385316468749999252, -29.71354166632526983, -3.109213912904139399 ) ) ;
#4034 = CARTESIAN_POINT ( 'NONE',  ( 1.467888652719048226, -4.549340926099360694, -3.492485675378536047 ) ) ;
#4035 = CARTESIAN_POINT ( 'NONE',  ( 2.841254879263533262, -6.049340926099361582, -2.815599370228847320 ) ) ;
#4036 = ORIENTED_EDGE ( 'NONE', *, *, #2707, .T. ) ;
#4037 = CIRCLE ( 'NONE', #4321, 1.499999999999999778 ) ;
#4038 = APPLICATION_CONTEXT ( 'automotive_design' ) ;
#4039 = CARTESIAN_POINT ( 'NONE',  ( -1.406733260263391960, -27.44866454968463287, 5.250000000000000000 ) ) ;
#4040 = CARTESIAN_POINT ( 'NONE',  ( 2.625000000000000444, -28.48958333401612819, -4.546633369868303021 ) ) ;
#4041 = CARTESIAN_POINT ( 'NONE',  ( 1.142306659890740623E-15, -29.79687499965859843, 6.218427825808274356 ) ) ;
#4042 = ORIENTED_EDGE ( 'NONE', *, *, #3134, .F. ) ;
#4043 = CARTESIAN_POINT ( 'NONE',  ( 2.692658234374998738, -27.66145833299193413, -4.663820869356206877 ) ) ;
#4044 = CARTESIAN_POINT ( 'NONE',  ( -1.431606283892693066, -3.250659073900639129, 3.507514324621434199 ) ) ;
#4045 = CARTESIAN_POINT ( 'NONE',  ( 6.972266317189433020E-16, -29.43750000000000000, -5.250000000000000000 ) ) ;
#4046 =( LENGTH_UNIT ( ) NAMED_UNIT ( * ) SI_UNIT ( .MILLI., .METRE. ) );
#4047 = CARTESIAN_POINT ( 'NONE',  ( -5.249999999999997335, -28.41666666598386826, 3.031088913245538308 ) ) ;
#4048 = CYLINDRICAL_SURFACE ( 'NONE', #6897, 2.549999999999999822 ) ;
#4049 = CARTESIAN_POINT ( 'NONE',  ( 0.000000000000000000, -27.00000000000000000, -5.250000000000000000 ) ) ;
#4050 = APPLICATION_PROTOCOL_DEFINITION ( 'draft international standard', 'automotive_design', 1998, #2427 ) ;
#4051 = CARTESIAN_POINT ( 'NONE',  ( 5.385316468750000141, -29.45312499965859843, -6.595110575850215044E-16 ) ) ;
#4052 = CARTESIAN_POINT ( 'NONE',  ( -1.431606283892620235, -4.749340926099363536, -3.507514324621463953 ) ) ;
#4053 = CARTESIAN_POINT ( 'NONE',  ( 0.000000000000000000, -30.00000000000000000, 5.250000000000000000 ) ) ;
#4054 = CARTESIAN_POINT ( 'NONE',  ( -5.385316468749998364, -29.30729166632526983, 3.109213912904140287 ) ) ;
#4055 = CARTESIAN_POINT ( 'NONE',  ( -1.467888652718973619, -5.850659073900639662, -3.492485675378565801 ) ) ;
#4056 = ORIENTED_EDGE ( 'NONE', *, *, #2297, .T. ) ;
#4057 = CARTESIAN_POINT ( 'NONE',  ( -1.406733260263385521, -27.10491455036742536, 5.250000000000006217 ) ) ;
#4058 = CARTESIAN_POINT ( 'NONE',  ( 5.182341765625000818, -26.96093750017070079, 0.000000000000000000 ) ) ;
#4059 = CARTESIAN_POINT ( 'NONE',  ( 1.467888652718972731, -5.050659073900638951, 3.492485675378566246 ) ) ;
#4060 = EDGE_LOOP ( 'NONE', ( #5251, #7001 ) ) ;
#4061 = CARTESIAN_POINT ( 'NONE',  ( -5.250000000000000000, -28.00000000000000000, 0.000000000000000000 ) ) ;
#4062 = ORIENTED_EDGE ( 'NONE', *, *, #8843, .T. ) ;
#4063 = CARTESIAN_POINT ( 'NONE',  ( -2.557341765625002594, -28.19270833367473017, 4.429445870380399164 ) ) ;
#4064 = CARTESIAN_POINT ( 'NONE',  ( 3.000000000000000444, -4.249340926099360871, 0.01814118441320859698 ) ) ;
#4065 = DIRECTION ( 'NONE',  ( 0.000000000000000000, -1.000000000000000000, 0.000000000000000000 ) ) ;
#4066 = CARTESIAN_POINT ( 'NONE',  ( -5.114683531249999859, -28.06770833367473017, -2.952963913586935440 ) ) ;
#4067 = PLANE ( 'NONE',  #8072 ) ;
#4068 = ADVANCED_FACE ( 'NONE', ( #5018 ), #7314, .T. ) ;
#4069 = CARTESIAN_POINT ( 'NONE',  ( 1.185285273922203525E-14, -28.96875000068279959, -5.249999999999999112 ) ) ;
#4070 = CARTESIAN_POINT ( 'NONE',  ( 2.300847884672513123E-14, -28.43750000000000000, -5.250000000000000000 ) ) ;
#4071 = CARTESIAN_POINT ( 'NONE',  ( -5.114683531250000748, -29.02604166700806587, 2.952963913586931888 ) ) ;
#4072 = ADVANCED_FACE ( 'NONE', ( #2906 ), #8567, .T. ) ;
#4073 = CARTESIAN_POINT ( 'NONE',  ( -6.972266317189433020E-16, -29.81250000000000000, -5.249999999999999112 ) ) ;
#4074 = CARTESIAN_POINT ( 'NONE',  ( 2.692658234375002735, -28.52604166632526628, 4.663820869356205101 ) ) ;
#4075 = CARTESIAN_POINT ( 'NONE',  ( -5.385316468750000141, -29.85937499965859843, 0.000000000000000000 ) ) ;
#4076 = AXIS2_PLACEMENT_3D ( 'NONE', #3353, #5431, #1208 ) ;
#4077 = DIRECTION ( 'NONE',  ( 0.000000000000000000, 0.000000000000000000, 1.000000000000000000 ) ) ;
#4078 = CARTESIAN_POINT ( 'NONE',  ( 1.142306659890740623E-15, -29.04687499965859843, 6.218427825808274356 ) ) ;
#4079 = CARTESIAN_POINT ( 'NONE',  ( 3.500000000000000000, -5.849340926099361404, 0.01814118441321387054 ) ) ;
#4080 = CARTESIAN_POINT ( 'NONE',  ( -0.01814118441321365544, -0.6493409260993610044, 3.500000000000000000 ) ) ;
#4081 = ORIENTED_EDGE ( 'NONE', *, *, #1054, .T. ) ;
#4082 = EDGE_CURVE ( 'NONE', #8842, #3705, #5116, .T. ) ;
#4083 = CYLINDRICAL_SURFACE ( 'NONE', #2996, 6.250000000000000000 ) ;
#4084 = CARTESIAN_POINT ( 'NONE',  ( 5.250000000000000000, -28.28125000068279604, 0.000000000000000000 ) ) ;
#4085 = CARTESIAN_POINT ( 'NONE',  ( 2.692658234375002735, -28.77604166632526628, 4.663820869356205101 ) ) ;
#4086 = ORIENTED_EDGE ( 'NONE', *, *, #6301, .F. ) ;
#4087 = CARTESIAN_POINT ( 'NONE',  ( -2.692658234375000514, -28.36979166632526628, -4.663820869356205989 ) ) ;
#4088 = CARTESIAN_POINT ( 'NONE',  ( 0.01814118441314514080, -6.550659073900640728, 3.000000000000000444 ) ) ;
#4089 = CARTESIAN_POINT ( 'NONE',  ( 0.000000000000000000, -30.00000000000000000, 0.000000000000000000 ) ) ;
#4090 = FACE_OUTER_BOUND ( 'NONE', #3004, .T. ) ;
#4091 = PLANE ( 'NONE',  #4935 ) ;
#4092 = CARTESIAN_POINT ( 'NONE',  ( -2.462045979635576920, -6.449340926099361937, -2.487701488670255756 ) ) ;
#4093 = LINE ( 'NONE', #5289, #8080 ) ;
#4094 = CARTESIAN_POINT ( 'NONE',  ( 2.033577675846918216E-14, -27.59375000068279959, 5.250000000000000888 ) ) ;
#4095 = APPLICATION_PROTOCOL_DEFINITION ( 'draft international standard', 'automotive_design', 1998, #3383 ) ;
#4096 = CARTESIAN_POINT ( 'NONE',  ( -5.385316468750000141, -29.07812499965860198, 0.000000000000000000 ) ) ;
#4097 = EDGE_CURVE ( 'NONE', #7275, #3705, #3033, .T. ) ;
#4098 = CARTESIAN_POINT ( 'NONE',  ( -3.507514324621464397, -5.149340926099360338, 1.431606283892619347 ) ) ;
#4099 = CARTESIAN_POINT ( 'NONE',  ( -1.406733260263391960, -29.44866454968462932, 5.250000000000000000 ) ) ;
#4100 = CARTESIAN_POINT ( 'NONE',  ( 1.142306659890740623E-15, -27.29687499965859843, 6.218427825808274356 ) ) ;
#4101 = EDGE_CURVE ( 'NONE', #5172, #3205, #89, .T. ) ;
#4102 = CARTESIAN_POINT ( 'NONE',  ( 1.638713065079247855, -5.650659073900638596, -4.007514324621431534 ) ) ;
#4103 = CARTESIAN_POINT ( 'NONE',  ( 0.000000000000000000, -9.999999999999998224, 0.000000000000000000 ) ) ;
#4104 = CARTESIAN_POINT ( 'NONE',  ( 0.000000000000000000, -30.00000000000000000, 0.000000000000000000 ) ) ;
#4105 = ORIENTED_EDGE ( 'NONE', *, *, #3064, .T. ) ;
#4106 = CARTESIAN_POINT ( 'NONE',  ( 2.625000000000002220, -28.41666666666666785, 4.546633369868302132 ) ) ;
#4107 = CARTESIAN_POINT ( 'NONE',  ( -5.114683531250000748, -27.25520833367473017, -2.952963913586935440 ) ) ;
#4108 = CARTESIAN_POINT ( 'NONE',  ( -1.224499502706077880, -4.749340926099361759, -3.007514324621463064 ) ) ;
#4109 = CARTESIAN_POINT ( 'NONE',  ( 2.624999999999998668, -28.08333333333333215, -4.546633369868303021 ) ) ;
#4110 = CARTESIAN_POINT ( 'NONE',  ( -2.624999999999998668, -29.91666666666666430, -4.546633369868303021 ) ) ;
#4111 = CARTESIAN_POINT ( 'NONE',  ( 0.000000000000000000, -53.00000000000000000, 1.749999999999999778 ) ) ;
#4112 = CARTESIAN_POINT ( 'NONE',  ( -2.557341765624999042, -29.58854166700806232, -4.429445870380400052 ) ) ;
#4113 = CARTESIAN_POINT ( 'NONE',  ( 5.114683531249998971, -28.94270833367473017, 2.952963913586936329 ) ) ;
#4114 = CARTESIAN_POINT ( 'NONE',  ( 0.000000000000000000, -27.00000000000000000, 0.000000000000000000 ) ) ;
#4115 = CARTESIAN_POINT ( 'NONE',  ( -5.249999999999999112, -28.66666666598386470, 3.031088913245538308 ) ) ;
#4116 = CARTESIAN_POINT ( 'NONE',  ( -5.385316468750001029, -29.63020833299193768, -3.109213912904136734 ) ) ;
#4117 = CARTESIAN_POINT ( 'NONE',  ( -1.975475456537005874E-15, -28.84375000068279959, 5.250000000000000000 ) ) ;
#4118 = DIRECTION ( 'NONE',  ( -0.000000000000000000, -1.000000000000000000, -0.000000000000000000 ) ) ;
#4119 = CARTESIAN_POINT ( 'NONE',  ( -2.487701488670255312, -2.049340926099361582, 2.462045979635577808 ) ) ;
#4120 = CARTESIAN_POINT ( 'NONE',  ( 2.462045979635577364, -2.449340926099361049, 2.487701488670255312 ) ) ;
#4121 = ORIENTED_EDGE ( 'NONE', *, *, #5300, .T. ) ;
#4122 = CARTESIAN_POINT ( 'NONE',  ( -5.250000000000000000, -29.68749999931720041, 0.000000000000000000 ) ) ;
#4123 = CARTESIAN_POINT ( 'NONE',  ( -5.114683531250000748, -29.48437500034139802, -6.263680815196995234E-16 ) ) ;
#4124 = CARTESIAN_POINT ( 'NONE',  ( -5.385316468750000141, -28.60937499965860198, 0.000000000000000000 ) ) ;
#4125 = EDGE_CURVE ( 'NONE', #1074, #2779, #4917, .T. ) ;
#4126 = ORIENTED_EDGE ( 'NONE', *, *, #905, .T. ) ;
#4127 = CARTESIAN_POINT ( 'NONE',  ( -5.385316468749998364, -29.05729166632526983, 3.109213912904140287 ) ) ;
#4128 = CARTESIAN_POINT ( 'NONE',  ( 1.224499502706142273, -5.650659073900639484, -3.007514324621435531 ) ) ;
#4129 = CARTESIAN_POINT ( 'NONE',  ( 0.000000000000000000, -30.00000000000000000, 0.000000000000000000 ) ) ;
#4130 = AXIS2_PLACEMENT_3D ( 'NONE', #7996, #7344, #1577 ) ;
#4131 = SURFACE_STYLE_USAGE ( .BOTH. , #1864 ) ;
#4132 = CARTESIAN_POINT ( 'NONE',  ( 5.182341765625000818, -26.96093750017070079, 0.000000000000000000 ) ) ;
#4133 = ADVANCED_FACE ( 'NONE', ( #8558 ), #4422, .F. ) ;
#4134 = CARTESIAN_POINT ( 'NONE',  ( 3.500000000000000000, -7.449340926099361937, 0.01814118441321387054 ) ) ;
#4135 = CARTESIAN_POINT ( 'NONE',  ( -2.557341765625002594, -28.44270833367473017, 4.429445870380399164 ) ) ;
#4136 = CARTESIAN_POINT ( 'NONE',  ( 5.249999999999999112, -28.29166666598387181, -3.031088913245536975 ) ) ;
#4137 = APPLICATION_PROTOCOL_DEFINITION ( 'draft international standard', 'automotive_design', 1998, #2753 ) ;
#4138 = EDGE_CURVE ( 'NONE', #8220, #2054, #8303, .T. ) ;
#4139 = DIRECTION ( 'NONE',  ( 0.000000000000000000, 0.000000000000000000, 1.000000000000000000 ) ) ;
#4140 = CARTESIAN_POINT ( 'NONE',  ( 3.500000000000000000, -5.849340926099361404, 0.01814118441321387054 ) ) ;
#4141 = CARTESIAN_POINT ( 'NONE',  ( 0.000000000000000000, -27.00000000000000000, 0.000000000000000000 ) ) ;
#4142 = CARTESIAN_POINT ( 'NONE',  ( -5.385316468750001029, -27.38020833299193768, -3.109213912904136734 ) ) ;
#4143 = CARTESIAN_POINT ( 'NONE',  ( 2.815599370228907716, -0.7506590739006385737, -2.841254879263473310 ) ) ;
#4144 = CARTESIAN_POINT ( 'NONE',  ( 2.143131898507868544E-16, -46.00000000000000000, -1.750000000000000222 ) ) ;
#4145 = CARTESIAN_POINT ( 'NONE',  ( 0.000000000000000000, -30.00000000000000000, 5.250000000000000000 ) ) ;
#4146 =( BOUNDED_CURVE ( )  B_SPLINE_CURVE ( 2, ( #3855, #6678, #8777, #2267, #6633, #5889, #3113, #8728, #8683 ),
 .UNSPECIFIED., .F., .F. ) 
 B_SPLINE_CURVE_WITH_KNOTS ( ( 3, 2, 2, 2, 3 ),
 ( 0.5208333333333333703, 0.5277777777777777901, 0.5416666666666666297, 0.5555555555555555802, 0.5625000000000000000 ),
 .UNSPECIFIED. ) 
 CURVE ( )  GEOMETRIC_REPRESENTATION_ITEM ( )  RATIONAL_B_SPLINE_CURVE ( ( 0.9330127018922192983, 0.9330127018922198534, 1.000000000000000000, 0.8660254037844387076, 1.000000000000000000, 0.8660254037844387076, 1.000000000000000000, 0.9330127018922194093, 0.9330127018922194093 ) ) 
 REPRESENTATION_ITEM ( '' )  );
#4147 = VERTEX_POINT ( 'NONE', #789 ) ;
#4148 = CARTESIAN_POINT ( 'NONE',  ( 5.250000000000000000, -28.85416666666666785, -3.031088913245536531 ) ) ;
#4149 = VECTOR ( 'NONE', #4904, 1000.000000000000000 ) ;
#4150 = CARTESIAN_POINT ( 'NONE',  ( -5.114683531250001636, -27.71354166700806587, 2.952963913586931444 ) ) ;
#4151 = CARTESIAN_POINT ( 'NONE',  ( 2.134148098076978251, -6.049340926099361582, -2.108492589042307408 ) ) ;
#4152 = CARTESIAN_POINT ( 'NONE',  ( 3.616337804771879580E-16, -27.35937500034140157, -5.905927827173866440 ) ) ;
#4153 = CYLINDRICAL_SURFACE ( 'NONE', #3190, 4.250000000000000000 ) ;
#4154 = CARTESIAN_POINT ( 'NONE',  ( -2.557341765625002594, -28.75520833367473017, 4.429445870380399164 ) ) ;
#4155 = AXIS2_PLACEMENT_3D ( 'NONE', #8945, #4032, #6913 ) ;
#4156 = PRODUCT ( 'spring', 'spring', '', ( #364 ) ) ;
#4157 = CYLINDRICAL_SURFACE ( 'NONE', #6087, 3.000000000000000444 ) ;
#4158 = CARTESIAN_POINT ( 'NONE',  ( -2.557341765625002594, -28.75520833367473017, 4.429445870380399164 ) ) ;
#4159 =( GEOMETRIC_REPRESENTATION_CONTEXT ( 3 ) GLOBAL_UNCERTAINTY_ASSIGNED_CONTEXT ( ( #7422 ) ) GLOBAL_UNIT_ASSIGNED_CONTEXT ( ( #3997, #6778, #456 ) ) REPRESENTATION_CONTEXT ( 'NONE', 'WORKASPACE' ) );
#4160 = DIRECTION ( 'NONE',  ( 0.000000000000000000, 0.000000000000000000, -1.000000000000000000 ) ) ;
#4161 = ADVANCED_FACE ( 'NONE', ( #8698 ), #881, .T. ) ;
#4162 = CARTESIAN_POINT ( 'NONE',  ( 2.625000000000002220, -29.60416666598386826, 4.546633369868302132 ) ) ;
#4163 = LINE ( 'NONE', #100, #8380 ) ;
#4164 = FACE_OUTER_BOUND ( 'NONE', #5923, .T. ) ;
#4165 = CARTESIAN_POINT ( 'NONE',  ( -2.487701488670255312, -5.249340926099360871, 2.462045979635577808 ) ) ;
#4166 = CARTESIAN_POINT ( 'NONE',  ( 4.000000000000000000, -5.849340926099360516, 0.01814118441321914063 ) ) ;
#4167 = ORIENTED_EDGE ( 'NONE', *, *, #391, .F. ) ;
#4168 = CARTESIAN_POINT ( 'NONE',  ( -6.972266317189433020E-16, -27.56249999999999645, -5.250000000000000000 ) ) ;
#4169 = AXIS2_PLACEMENT_3D ( 'NONE', #8065, #2443, #8256 ) ;
#4170 = CARTESIAN_POINT ( 'NONE',  ( -2.557341765624999042, -29.27604166700806232, -4.429445870380400052 ) ) ;
#4171 = CARTESIAN_POINT ( 'NONE',  ( -2.625000000000000444, -27.22916666598386826, -4.546633369868303021 ) ) ;
#4172 = ORIENTED_EDGE ( 'NONE', *, *, #5831, .F. ) ;
#4173 = CARTESIAN_POINT ( 'NONE',  ( 2.692658234375002735, -29.24479166632526983, 4.663820869356205101 ) ) ;
#4174 = CARTESIAN_POINT ( 'NONE',  ( -4.000000000000000000, 0.2493409260993615095, 0.01814118441313491634 ) ) ;
#4175 = FACE_OUTER_BOUND ( 'NONE', #8554, .T. ) ;
#4176 = AXIS2_PLACEMENT_3D ( 'NONE', #4011, #7498, #5441 ) ;
#4177 = CARTESIAN_POINT ( 'NONE',  ( -1.406733260263382856, -27.67633545031536713, -5.250000000000006217 ) ) ;
#4178 = FACE_BOUND ( 'NONE', #5344, .T. ) ;
#4179 = DIRECTION ( 'NONE',  ( -0.000000000000000000, 1.000000000000000000, -0.000000000000000000 ) ) ;
#4180 = AXIS2_PLACEMENT_3D ( 'NONE', #1944, #1102, #1241 ) ;
#4181 = CARTESIAN_POINT ( 'NONE',  ( 5.114683531249998971, -28.63020833367472662, 2.952963913586936329 ) ) ;
#4182 = CARTESIAN_POINT ( 'NONE',  ( 2.625000000000002220, -28.35416666598386826, 4.546633369868302132 ) ) ;
#4183 = DIRECTION ( 'NONE',  ( -0.000000000000000000, 1.000000000000000000, -0.000000000000000000 ) ) ;
#4184 = CARTESIAN_POINT ( 'NONE',  ( -1.260781871532494103, -3.749340926099361315, 2.992485675378538712 ) ) ;
#4185 = CARTESIAN_POINT ( 'NONE',  ( 3.091560946453699876E-16, -20.00000000000000000, 2.000000000000000000 ) ) ;
#4186 = CARTESIAN_POINT ( 'NONE',  ( 5.385316468750001029, -29.97395833299194123, 3.109213912904135846 ) ) ;
#4187 = CARTESIAN_POINT ( 'NONE',  ( -1.638713065079245634, -4.850659073900639662, 4.007514324621432422 ) ) ;
#4188 = CARTESIAN_POINT ( 'NONE',  ( 5.249999999999999112, -28.97916666666666430, -3.031088913245534755 ) ) ;
#4189 =( NAMED_UNIT ( * ) SI_UNIT ( $, .STERADIAN. ) SOLID_ANGLE_UNIT ( ) );
#4190 = ADVANCED_FACE ( 'NONE', ( #3778 ), #7782, .T. ) ;
#4191 = CARTESIAN_POINT ( 'NONE',  ( -3.250000000000006661, -0.000000000000000000, 0.5527349658716841363 ) ) ;
#4192 = ORIENTED_EDGE ( 'NONE', *, *, #6309, .T. ) ;
#4193 = CARTESIAN_POINT ( 'NONE',  ( -2.692658234374996518, -27.28645833299193413, 4.663820869356208654 ) ) ;
#4194 = VERTEX_POINT ( 'NONE', #582 ) ;
#4195 = CARTESIAN_POINT ( 'NONE',  ( -5.114683531250000748, -27.00520833367473017, -2.952963913586935440 ) ) ;
#4196 = CARTESIAN_POINT ( 'NONE',  ( 2.134148098076978251, -7.649340926099361226, -2.108492589042307408 ) ) ;
#4197 = CARTESIAN_POINT ( 'NONE',  ( -5.114683531250000748, -28.04687500034139802, -6.263680815196995234E-16 ) ) ;
#4198 = CARTESIAN_POINT ( 'NONE',  ( 0.000000000000000000, 70.00000000000000000, 0.000000000000000000 ) ) ;
#4199 =( BOUNDED_CURVE ( )  B_SPLINE_CURVE ( 2, ( #9108, #4099, #1916, #1118, #1213, #2570, #6887, #8331, #5388 ),
 .UNSPECIFIED., .F., .F. ) 
 B_SPLINE_CURVE_WITH_KNOTS ( ( 3, 2, 2, 2, 3 ),
 ( 0.8125000000000000000, 0.8194444444444444198, 0.8333333333333333703, 0.8472222222222222099, 0.8541666666666667407 ),
 .UNSPECIFIED. ) 
 CURVE ( )  GEOMETRIC_REPRESENTATION_ITEM ( )  RATIONAL_B_SPLINE_CURVE ( ( 0.9330127018922194093, 0.9330127018922194093, 1.000000000000000000, 0.8660254037844387076, 1.000000000000000000, 0.8660254037844387076, 1.000000000000000000, 0.9330127018922187432, 0.9330127018922192983 ) ) 
 REPRESENTATION_ITEM ( '' )  );
#4200 = CARTESIAN_POINT ( 'NONE',  ( 3.616337804771879580E-16, -28.85937500034139802, -5.905927827173866440 ) ) ;
#4201 = VECTOR ( 'NONE', #3039, 1000.000000000000000 ) ;
#4202 = CARTESIAN_POINT ( 'NONE',  ( 2.557341765624996821, -28.21354166700806587, 4.429445870380401828 ) ) ;
#4203 = CARTESIAN_POINT ( 'NONE',  ( -2.324088772396477476E-15, -29.68750000000000000, -5.250000000000000000 ) ) ;
#4204 = CARTESIAN_POINT ( 'NONE',  ( 5.250000000000000888, -29.83333333265053966, 3.031088913245532979 ) ) ;
#4205 = CARTESIAN_POINT ( 'NONE',  ( 5.204748896376250699E-16, -9.999999999999998224, -4.250000000000000000 ) ) ;
#4206 = CARTESIAN_POINT ( 'NONE',  ( 0.000000000000000000, -9.000000000000000000, 5.750000000000000000 ) ) ;
#4207 = AXIS2_PLACEMENT_3D ( 'NONE', #5946, #8786, #2416 ) ;
#4208 = CARTESIAN_POINT ( 'NONE',  ( 6.429395695523604153E-16, -27.00000000000000000, 5.250000000000000000 ) ) ;
#4209 = CARTESIAN_POINT ( 'NONE',  ( 3.500000000000000000, -4.249340926099360871, 0.01814118441321387054 ) ) ;
#4210 = CARTESIAN_POINT ( 'NONE',  ( 3.492485675378536047, -5.749340926099363536, 1.467888652719046672 ) ) ;
#4211 = EDGE_CURVE ( 'NONE', #2331, #3224, #1368, .T. ) ;
#4212 = AXIS2_PLACEMENT_3D ( 'NONE', #3095, #8665, #6010 ) ;
#4213 = ORIENTED_EDGE ( 'NONE', *, *, #8224, .T. ) ;
#4214 = DIRECTION ( 'NONE',  ( 0.000000000000000000, -0.000000000000000000, 1.000000000000000000 ) ) ;
#4215 = CARTESIAN_POINT ( 'NONE',  ( -5.250000000000000888, -27.13541666734946389, 3.031088913245532979 ) ) ;
#4216 = VECTOR ( 'NONE', #5336, 1000.000000000000000 ) ;
#4217 = EDGE_LOOP ( 'NONE', ( #8444, #2232, #8112, #2391, #6761, #5078 ) ) ;
#4218 = CARTESIAN_POINT ( 'NONE',  ( -5.385316468750000141, -30.07812499965859843, 0.000000000000000000 ) ) ;
#4219 = CARTESIAN_POINT ( 'NONE',  ( 3.492485675378566690, -5.450659073900639306, -1.467888652718972287 ) ) ;
#4220 = CARTESIAN_POINT ( 'NONE',  ( 0.000000000000000000, -27.00000000000000000, -5.250000000000000000 ) ) ;
#4221 = EDGE_LOOP ( 'NONE', ( #3263, #2347, #5735, #1741 ) ) ;
#4222 = AXIS2_PLACEMENT_3D ( 'NONE', #8897, #5411, #1185 ) ;
#4223 = CARTESIAN_POINT ( 'NONE',  ( 6.429395695523604153E-16, -27.00000000000000000, 5.250000000000000000 ) ) ;
#4224 = LINE ( 'NONE', #771, #5318 ) ;
#4225 = DIRECTION ( 'NONE',  ( 0.000000000000000000, 0.000000000000000000, -1.000000000000000000 ) ) ;
#4226 = CARTESIAN_POINT ( 'NONE',  ( -5.114683531250000748, -29.23437500034139802, -6.263680815196995234E-16 ) ) ;
#4227 = DIRECTION ( 'NONE',  ( 0.000000000000000000, 0.000000000000000000, -1.000000000000000000 ) ) ;
#4228 = CONTEXT_DEPENDENT_SHAPE_REPRESENTATION ( #6572, #6979 ) ;
#4229 = CARTESIAN_POINT ( 'NONE',  ( 5.250000000000000888, -27.83333333265053611, 3.031088913245533423 ) ) ;
#4230 = CARTESIAN_POINT ( 'NONE',  ( 3.007514324621463508, -7.549340926099361582, -1.224499502706076770 ) ) ;
#4231 = CARTESIAN_POINT ( 'NONE',  ( 0.000000000000000000, -30.00000000000000000, 0.000000000000000000 ) ) ;
#4232 = CARTESIAN_POINT ( 'NONE',  ( 1.142306659890740623E-15, -29.26562499965860198, 6.218427825808274356 ) ) ;
#4233 = EDGE_CURVE ( 'NONE', #2823, #451, #5978, .T. ) ;
#4234 = CARTESIAN_POINT ( 'NONE',  ( -4.000000000000000000, -1.350659073900638552, 0.01814118441313491634 ) ) ;
#4235 = PLANE ( 'NONE',  #7884 ) ;
#4236 = CARTESIAN_POINT ( 'NONE',  ( -5.249999999999999112, -26.92708333401612819, -3.031088913245536975 ) ) ;
#4237 = ADVANCED_FACE ( 'NONE', ( #1450 ), #4251, .F. ) ;
#4238 = EDGE_LOOP ( 'NONE', ( #1631, #1106, #1651, #5055 ) ) ;
#4239 = CARTESIAN_POINT ( 'NONE',  ( -3.712013335537174572E-16, -29.31249999999999645, -6.062177826491070398 ) ) ;
#4240 = CARTESIAN_POINT ( 'NONE',  ( -2.557341765625002594, -27.19270833367473017, 4.429445870380399164 ) ) ;
#4241 = CARTESIAN_POINT ( 'NONE',  ( -1.260781871532494103, -5.349340926099361404, 2.992485675378538712 ) ) ;
#4242 = CARTESIAN_POINT ( 'NONE',  ( 3.712013335537174572E-16, -29.68750000000000000, -6.062177826491070398 ) ) ;
#4243 = FACE_BOUND ( 'NONE', #1146, .T. ) ;
#4244 = CARTESIAN_POINT ( 'NONE',  ( -5.114683531250001636, -29.02604166700806587, 2.952963913586931444 ) ) ;
#4245 = CARTESIAN_POINT ( 'NONE',  ( 5.114683531249998971, -27.19270833367473017, 2.952963913586936329 ) ) ;
#4246 = CARTESIAN_POINT ( 'NONE',  ( -5.250000000000000000, -28.40625000068279604, -6.429395695523604153E-16 ) ) ;
#4247 = CARTESIAN_POINT ( 'NONE',  ( 5.250000000000000888, -29.08333333265053611, 3.031088913245532979 ) ) ;
#4248 =( BOUNDED_CURVE ( )  B_SPLINE_CURVE ( 2, ( #6207, #8396, #1407, #577, #663, #9166, #6910, #5636, #6949 ),
 .UNSPECIFIED., .F., .F. ) 
 B_SPLINE_CURVE_WITH_KNOTS ( ( 3, 2, 2, 2, 3 ),
 ( 0.7291666666666667407, 0.7361111111111111605, 0.7500000000000000000, 0.7638888888888888395, 0.7708333333333333703 ),
 .UNSPECIFIED. ) 
 CURVE ( )  GEOMETRIC_REPRESENTATION_ITEM ( )  RATIONAL_B_SPLINE_CURVE ( ( 0.9330127018922192983, 0.9330127018922198534, 1.000000000000000000, 0.8660254037844387076, 1.000000000000000000, 0.8660254037844387076, 1.000000000000000000, 0.9330127018922187432, 0.9330127018922192983 ) ) 
 REPRESENTATION_ITEM ( '' )  );
#4249 = DIRECTION ( 'NONE',  ( 0.000000000000000000, 0.000000000000000000, 1.000000000000000000 ) ) ;
#4250 = CARTESIAN_POINT ( 'NONE',  ( -1.971654945569944140, -3.316496963571793567E-17, 2.933326779092722436 ) ) ;
#4251 = PLANE ( 'NONE',  #4502 ) ;
#4252 = CARTESIAN_POINT ( 'NONE',  ( -1.975475456537005874E-15, -29.59375000068279249, 5.250000000000000000 ) ) ;
#4253 = CARTESIAN_POINT ( 'NONE',  ( -3.500000000000000000, -3.449340926099361049, -0.01814118441321344033 ) ) ;
#4254 = ORIENTED_EDGE ( 'NONE', *, *, #5831, .T. ) ;
#4255 = CARTESIAN_POINT ( 'NONE',  ( 5.249999999999999112, -27.30208333401612819, 3.031088913245538308 ) ) ;
#4256 = ADVANCED_FACE ( 'NONE', ( #6376, #2864 ), #3466, .F. ) ;
#4257 = ORIENTED_EDGE ( 'NONE', *, *, #3723, .T. ) ;
#4258 = CARTESIAN_POINT ( 'NONE',  ( -2.692658234374996518, -29.03645833299193413, 4.663820869356208654 ) ) ;
#4259 = CARTESIAN_POINT ( 'NONE',  ( 2.462045979635629767, -3.950659073900639751, -2.487701488670203354 ) ) ;
#4260 = LINE ( 'NONE', #767, #8895 ) ;
#4261 = VERTEX_POINT ( 'NONE', #3511 ) ;
#4262 = PRODUCT_DEFINITION_SHAPE ( 'NONE', 'NONE',  #741 ) ;
#4263 = CARTESIAN_POINT ( 'NONE',  ( 0.000000000000000000, -50.00000000000000000, 0.000000000000000000 ) ) ;
#4264 = CARTESIAN_POINT ( 'NONE',  ( 0.000000000000000000, -20.00000000000000000, 0.000000000000000000 ) ) ;
#4265 = CARTESIAN_POINT ( 'NONE',  ( 5.250000000000000000, -28.87499999999999645, -6.429395695523604153E-16 ) ) ;
#4266 = CARTESIAN_POINT ( 'NONE',  ( -5.114683531250000748, -28.46354166700806587, 2.952963913586931888 ) ) ;
#4267 = DIRECTION ( 'NONE',  ( 0.000000000000000000, -1.000000000000000000, 0.000000000000000000 ) ) ;
#4268 = CARTESIAN_POINT ( 'NONE',  ( 5.250000000000000000, -29.03125000068279604, 0.000000000000000000 ) ) ;
#4269 = CARTESIAN_POINT ( 'NONE',  ( 2.134148098076978251, -4.449340926099361937, -2.108492589042307408 ) ) ;
#4270 = CARTESIAN_POINT ( 'NONE',  ( 1.000000000000000000, -29.00000000000000355, -3.048902179152658931 ) ) ;
#4271 =( BOUNDED_CURVE ( )  B_SPLINE_CURVE ( 2, ( #2157, #7832, #2111, #4893, #5555, #6295, #6423, #7131, #753 ),
 .UNSPECIFIED., .F., .T. ) 
 B_SPLINE_CURVE_WITH_KNOTS ( ( 3, 2, 2, 2, 3 ),
 ( 0.4791666666666666852, 0.4861111111111111049, 0.5000000000000000000, 0.5138888888888888395, 0.5208333333333332593 ),
 .UNSPECIFIED. ) 
 CURVE ( )  GEOMETRIC_REPRESENTATION_ITEM ( )  RATIONAL_B_SPLINE_CURVE ( ( 0.9330127018922194093, 0.9330127018922196314, 1.000000000000000000, 0.8660254037844387076, 1.000000000000000000, 0.8660254037844387076, 1.000000000000000000, 0.9330127018922198534, 0.9330127018922192983 ) ) 
 REPRESENTATION_ITEM ( '' )  );
#4272 = STYLED_ITEM ( 'NONE', ( #6150 ), #3635 ) ;
#4273 = VECTOR ( 'NONE', #637, 1000.000000000000000 ) ;
#4274 = CARTESIAN_POINT ( 'NONE',  ( 2.692658234374998738, -27.44270833299193413, -4.663820869356206877 ) ) ;
#4275 = ADVANCED_FACE ( 'NONE', ( #2909 ), #5683, .T. ) ;
#4276 = CARTESIAN_POINT ( 'NONE',  ( 2.841254879263473310, -1.950659073900638640, 2.815599370228907272 ) ) ;
#4277 = SURFACE_STYLE_USAGE ( .BOTH. , #649 ) ;
#4278 = LINE ( 'NONE', #7246, #2690 ) ;
#4279 = MECHANICAL_DESIGN_GEOMETRIC_PRESENTATION_REPRESENTATION (  '', ( #2499 ), #6348 ) ;
#4280 = ORIENTED_EDGE ( 'NONE', *, *, #5363, .F. ) ;
#4281 = SURFACE_STYLE_FILL_AREA ( #2 ) ;
#4282 = CARTESIAN_POINT ( 'NONE',  ( 2.625000000000002220, -29.16666666666666785, 4.546633369868302132 ) ) ;
#4283 = DIRECTION ( 'NONE',  ( 0.000000000000000000, 0.000000000000000000, -1.000000000000000000 ) ) ;
#4284 = CARTESIAN_POINT ( 'NONE',  ( 1.260781871532430598, -0.2506590739006394064, 2.992485675378564469 ) ) ;
#4285 = EDGE_LOOP ( 'NONE', ( #4086, #5177, #8194, #86 ) ) ;
#4286 = CARTESIAN_POINT ( 'NONE',  ( -5.250000000000000000, -29.62500000000000000, -6.429395695523604153E-16 ) ) ;
#4287 = DIRECTION ( 'NONE',  ( -0.000000000000000000, 1.000000000000000000, -0.000000000000000000 ) ) ;
#4288 = CARTESIAN_POINT ( 'NONE',  ( 2.557341765625000818, -29.13020833367473017, -4.429445870380400052 ) ) ;
#4289 = SURFACE_STYLE_USAGE ( .BOTH. , #2194 ) ;
#4290 = CARTESIAN_POINT ( 'NONE',  ( -5.114683531249999859, -27.56770833367473017, -2.952963913586935440 ) ) ;
#4291 = CARTESIAN_POINT ( 'NONE',  ( -5.250000000000000000, -29.68749999931720041, 0.000000000000000000 ) ) ;
#4292 = CARTESIAN_POINT ( 'NONE',  ( -1.000000000000000000, -30.99986970103996953, -2.582962878832828046 ) ) ;
#4293 = PRESENTATION_STYLE_ASSIGNMENT (( #2818 ) ) ;
#4294 = DIRECTION ( 'NONE',  ( 0.000000000000000000, 0.000000000000000000, -1.000000000000000000 ) ) ;
#4295 = CARTESIAN_POINT ( 'NONE',  ( 5.114683531250000748, -29.92187500034139802, 0.000000000000000000 ) ) ;
#4296 = CARTESIAN_POINT ( 'NONE',  ( 3.507514324621465285, -5.949340926099361937, -1.431606283892619125 ) ) ;
#4297 = ORIENTED_EDGE ( 'NONE', *, *, #1607, .T. ) ;
#4298 = AXIS2_PLACEMENT_3D ( 'NONE', #8181, #6074, #8911 ) ;
#4299 = CARTESIAN_POINT ( 'NONE',  ( -1.431606283892693066, -6.450659073900639306, 3.507514324621434199 ) ) ;
#4300 = CARTESIAN_POINT ( 'NONE',  ( -1.406733260263384411, -29.73883544963257108, -5.250000000000006217 ) ) ;
#4301 = CARTESIAN_POINT ( 'NONE',  ( 5.250000000000000000, -27.01041666734946389, -3.031088913245534755 ) ) ;
#4302 = EDGE_CURVE ( 'NONE', #4375, #2122, #3320, .T. ) ;
#4303 = ORIENTED_EDGE ( 'NONE', *, *, #885, .T. ) ;
#4304 = ORIENTED_EDGE ( 'NONE', *, *, #4479, .T. ) ;
#4305 = AXIS2_PLACEMENT_3D ( 'NONE', #8307, #4677, #1098 ) ;
#4306 = CARTESIAN_POINT ( 'NONE',  ( -5.385316468750001029, -29.84895833299193413, -3.109213912904136734 ) ) ;
#4307 = CARTESIAN_POINT ( 'NONE',  ( -1.467888652718973619, -7.450659073900638418, -3.492485675378565801 ) ) ;
#4308 = FACE_BOUND ( 'NONE', #4309, .T. ) ;
#4309 = EDGE_LOOP ( 'NONE', ( #2941, #2473 ) ) ;
#4310 = AXIS2_PLACEMENT_3D ( 'NONE', #8017, #1695, #5778 ) ;
#4311 = CARTESIAN_POINT ( 'NONE',  ( -2.033577675846918216E-14, -28.93750000000000000, 5.250000000000000888 ) ) ;
#4312 = CARTESIAN_POINT ( 'NONE',  ( 1.000000000000000000, -30.99986970103996953, -2.582962878832828046 ) ) ;
#4313 = CARTESIAN_POINT ( 'NONE',  ( 5.385316468749999252, -27.21354166632526628, -3.109213912904139399 ) ) ;
#4314 = CARTESIAN_POINT ( 'NONE',  ( -5.114683531250000748, -28.98437500034139802, -6.263680815196995234E-16 ) ) ;
#4315 = CARTESIAN_POINT ( 'NONE',  ( 5.249999999999999112, -27.51041666734946389, -3.031088913245534755 ) ) ;
#4316 = DIRECTION ( 'NONE',  ( 0.000000000000000000, 1.000000000000000000, 0.000000000000000000 ) ) ;
#4317 = CARTESIAN_POINT ( 'NONE',  ( 3.007514324621463508, -5.949340926099362825, -1.224499502706076770 ) ) ;
#4318 = CARTESIAN_POINT ( 'NONE',  ( 0.000000000000000000, -20.00000000000000000, 0.000000000000000000 ) ) ;
#4319 = CARTESIAN_POINT ( 'NONE',  ( 1.142306659890740623E-15, -27.79687499965860198, 6.218427825808274356 ) ) ;
#4320 = CARTESIAN_POINT ( 'NONE',  ( 2.815599370228847320, -2.449340926099361049, 2.841254879263533262 ) ) ;
#4321 = AXIS2_PLACEMENT_3D ( 'NONE', #4747, #3265, #521 ) ;
#4322 = CARTESIAN_POINT ( 'NONE',  ( 2.033577675846918216E-14, -27.31250000000000000, 5.250000000000000888 ) ) ;
#4323 = APPLICATION_CONTEXT ( 'automotive_design' ) ;
#4324 = CARTESIAN_POINT ( 'NONE',  ( -1.406733260263385521, -27.60491455036742181, 5.250000000000006217 ) ) ;
#4325 = ORIENTED_EDGE ( 'NONE', *, *, #3227, .F. ) ;
#4326 =( BOUNDED_CURVE ( )  B_SPLINE_CURVE ( 2, ( #6482, #8632, #8816, #4402, #5231, #8076, #7232, #1753, #1605 ),
 .UNSPECIFIED., .F., .T. ) 
 B_SPLINE_CURVE_WITH_KNOTS ( ( 3, 2, 2, 2, 3 ),
 ( 0.02083333333333333218, 0.02777777777777777624, 0.04166666666666666435, 0.05555555555555555247, 0.06250000000000000000 ),
 .UNSPECIFIED. ) 
 CURVE ( )  GEOMETRIC_REPRESENTATION_ITEM ( )  RATIONAL_B_SPLINE_CURVE ( ( 0.9330127018922194093, 0.9330127018922194093, 1.000000000000000000, 0.8660254037844387076, 1.000000000000000000, 0.8660254037844387076, 1.000000000000000000, 0.9330127018922194093, 0.9330127018922194093 ) ) 
 REPRESENTATION_ITEM ( '' )  );
#4327 = CARTESIAN_POINT ( 'NONE',  ( -5.385316468750000141, -27.32812499965860198, 0.000000000000000000 ) ) ;
#4328 = ORIENTED_EDGE ( 'NONE', *, *, #5626, .T. ) ;
#4329 = CARTESIAN_POINT ( 'NONE',  ( -2.557341765625002594, -26.94270833367473017, 4.429445870380399164 ) ) ;
#4330 = CARTESIAN_POINT ( 'NONE',  ( -3.007514324621463508, -6.749340926099361759, 1.224499502706077658 ) ) ;
#4331 = PRODUCT_DEFINITION ( 'UNKNOWN', '', #565, #220 ) ;
#4332 = ORIENTED_EDGE ( 'NONE', *, *, #5112, .T. ) ;
#4333 = CARTESIAN_POINT ( 'NONE',  ( -2.624999999999998668, -28.66666666666666785, -4.546633369868303021 ) ) ;
#4334 = CYLINDRICAL_SURFACE ( 'NONE', #4517, 3.000000000000000444 ) ;
#4335 = CARTESIAN_POINT ( 'NONE',  ( -1.084901341431563726E-15, -28.23437500034139447, 5.905927827173866440 ) ) ;
#4336 = CARTESIAN_POINT ( 'NONE',  ( 5.114683531249999859, -28.15104166700806587, -2.952963913586932776 ) ) ;
#4337 = CARTESIAN_POINT ( 'NONE',  ( -5.250000000000000000, -29.93749999931720041, 0.000000000000000000 ) ) ;
#4338 = DIRECTION ( 'NONE',  ( 0.000000000000000000, 1.000000000000000000, 0.000000000000000000 ) ) ;
#4339 = CYLINDRICAL_SURFACE ( 'NONE', #1628, 5.250000000000000000 ) ;
#4340 = CARTESIAN_POINT ( 'NONE',  ( 1.975475456537005874E-15, -27.68749999999999289, 5.250000000000000000 ) ) ;
#4341 = CARTESIAN_POINT ( 'NONE',  ( 2.557341765624996821, -29.71354166700806232, 4.429445870380401828 ) ) ;
#4342 = CARTESIAN_POINT ( 'NONE',  ( 2.462045979635577364, -5.649340926099361226, 2.487701488670255312 ) ) ;
#4343 = ADVANCED_FACE ( 'NONE', ( #1279 ), #2775, .T. ) ;
#4344 = ORIENTED_EDGE ( 'NONE', *, *, #5766, .F. ) ;
#4345 = CARTESIAN_POINT ( 'NONE',  ( -5.250000000000000000, -28.65625000068279604, -6.429395695523604153E-16 ) ) ;
#4346 = CARTESIAN_POINT ( 'NONE',  ( 0.000000000000000000, -20.00000000000000000, 0.000000000000000000 ) ) ;
#4347 = CARTESIAN_POINT ( 'NONE',  ( 5.114683531249998971, -27.88020833367473017, 2.952963913586936329 ) ) ;
#4348 = EDGE_CURVE ( 'NONE', #8645, #8220, #4271, .T. ) ;
#4349 = EDGE_LOOP ( 'NONE', ( #6694, #6748 ) ) ;
#4350 = VERTEX_POINT ( 'NONE', #3598 ) ;
#4351 = EDGE_CURVE ( 'NONE', #301, #7570, #60, .T. ) ;
#4352 = CARTESIAN_POINT ( 'NONE',  ( -5.249999999999997335, -29.72916666666666430, 3.031088913245538308 ) ) ;
#4353 = CARTESIAN_POINT ( 'NONE',  ( 5.385316468749999252, -27.46354166632526628, -3.109213912904138954 ) ) ;
#4354 = CARTESIAN_POINT ( 'NONE',  ( -3.507514324621434199, -4.450659073900639306, -1.431606283892695064 ) ) ;
#4355 = VECTOR ( 'NONE', #6243, 1000.000000000000000 ) ;
#4356 = LINE ( 'NONE', #997, #8596 ) ;
#4357 = ORIENTED_EDGE ( 'NONE', *, *, #1575, .T. ) ;
#4358 = LINE ( 'NONE', #6349, #467 ) ;
#4359 = CARTESIAN_POINT ( 'NONE',  ( 5.249999999999999112, -29.30208333401613174, 3.031088913245538308 ) ) ;
#4360 = DIRECTION ( 'NONE',  ( 0.000000000000000000, 0.000000000000000000, 1.000000000000000000 ) ) ;
#4361 = PRESENTATION_LAYER_ASSIGNMENT (  '', '', ( #1097 ) ) ;
#4362 = CARTESIAN_POINT ( 'NONE',  ( -1.084901341431563923E-15, -27.42187500034139802, 5.905927827173866440 ) ) ;
#4363 = DIRECTION ( 'NONE',  ( 0.000000000000000000, 1.000000000000000000, 0.000000000000000000 ) ) ;
#4364 = CARTESIAN_POINT ( 'NONE',  ( -3.807688866302469071E-16, -27.14062499965860198, -6.218427825808274356 ) ) ;
#4365 = CARTESIAN_POINT ( 'NONE',  ( 1.260781871532495657, -1.349340926099361626, -2.992485675378538268 ) ) ;
#4366 = CARTESIAN_POINT ( 'NONE',  ( -3.807688866302469071E-16, -27.67187499965859843, -6.218427825808274356 ) ) ;
#4367 = CARTESIAN_POINT ( 'NONE',  ( 1.674995433905601239, -4.549340926099363358, -3.992485675378532939 ) ) ;
#4368 = AXIS2_PLACEMENT_3D ( 'NONE', #3258, #6083, #8919 ) ;
#4369 = DIRECTION ( 'NONE',  ( -0.000000000000000000, 1.000000000000000000, -0.000000000000000000 ) ) ;
#4370 = DIRECTION ( 'NONE',  ( 0.000000000000000000, -0.9973637043974449279, -0.07256473765270717025 ) ) ;
#4371 = EDGE_CURVE ( 'NONE', #5007, #3199, #1678, .T. ) ;
#4372 = CYLINDRICAL_SURFACE ( 'NONE', #4455, 5.250000000000000000 ) ;
#4373 = ORIENTED_EDGE ( 'NONE', *, *, #4416, .T. ) ;
#4374 = CARTESIAN_POINT ( 'NONE',  ( -5.250000000000000000, -29.27083333333333215, -3.031088913245534755 ) ) ;
#4375 = VERTEX_POINT ( 'NONE', #666 ) ;
#4376 = CARTESIAN_POINT ( 'NONE',  ( 2.692658234375002735, -27.49479166632526628, 4.663820869356205101 ) ) ;
#4377 = CARTESIAN_POINT ( 'NONE',  ( -1.224499502706140497, -4.850659073900639662, 3.007514324621436863 ) ) ;
#4378 = VERTEX_POINT ( 'NONE', #8489 ) ;
#4379 = CARTESIAN_POINT ( 'NONE',  ( 2.624999999999996891, -29.29166666666666785, 4.546633369868304797 ) ) ;
#4380 = DIRECTION ( 'NONE',  ( 0.000000000000000000, 0.000000000000000000, 1.000000000000000000 ) ) ;
#4381 = CARTESIAN_POINT ( 'NONE',  ( 5.114683531250000748, -28.40104166700806587, -2.952963913586932776 ) ) ;
#4382 = PRESENTATION_STYLE_ASSIGNMENT (( #1405 ) ) ;
#4383 = CARTESIAN_POINT ( 'NONE',  ( 5.114683531249998971, -27.94270833367473017, 2.952963913586936329 ) ) ;
#4384 = SHAPE_REPRESENTATION ( 'dispenser ring', ( #888 ), #1745 ) ;
#4385 = LINE ( 'NONE', #7215, #1038 ) ;
#4386 = CARTESIAN_POINT ( 'NONE',  ( 2.487701488670255756, -2.849340926099361404, -2.462045979635577364 ) ) ;
#4387 = CARTESIAN_POINT ( 'NONE',  ( 0.000000000000000000, 75.00000000000000000, 0.000000000000000000 ) ) ;
#4388 = CARTESIAN_POINT ( 'NONE',  ( -2.625000000000002220, -27.36458333401612819, 4.546633369868302132 ) ) ;
#4389 = FACE_OUTER_BOUND ( 'NONE', #3284, .T. ) ;
#4390 = CARTESIAN_POINT ( 'NONE',  ( -1.431606283892620235, -4.749340926099363536, -3.507514324621463953 ) ) ;
#4391 = EDGE_LOOP ( 'NONE', ( #3317, #2284, #6338, #3514 ) ) ;
#4392 = CARTESIAN_POINT ( 'NONE',  ( 2.624999999999998668, -27.08333333333333570, -4.546633369868303021 ) ) ;
#4393 = DIRECTION ( 'NONE',  ( -0.000000000000000000, -1.000000000000000000, -0.000000000000000000 ) ) ;
#4394 = CARTESIAN_POINT ( 'NONE',  ( 2.557341765624996821, -28.90104166700806587, 4.429445870380401828 ) ) ;
#4395 = VERTEX_POINT ( 'NONE', #2728 ) ;
#4396 = EDGE_LOOP ( 'NONE', ( #6921, #2276 ) ) ;
#4397 = DIRECTION ( 'NONE',  ( 0.000000000000000000, 1.000000000000000000, 0.000000000000000000 ) ) ;
#4398 = CARTESIAN_POINT ( 'NONE',  ( -1.674995433905599462, -0.5493409260993608045, 3.992485675378533383 ) ) ;
#4399 = CARTESIAN_POINT ( 'NONE',  ( 2.624999999999996891, -27.54166666666666430, 4.546633369868304797 ) ) ;
#4400 = ORIENTED_EDGE ( 'NONE', *, *, #5699, .T. ) ;
#4401 = EDGE_CURVE ( 'NONE', #7820, #8840, #6179, .T. ) ;
#4402 = CARTESIAN_POINT ( 'NONE',  ( -5.249999999999999112, -29.89583333333333215, -3.031088913245536975 ) ) ;
#4403 = CARTESIAN_POINT ( 'NONE',  ( 5.250000000000000000, -29.26041666734946389, -3.031088913245534755 ) ) ;
#4404 = CARTESIAN_POINT ( 'NONE',  ( -2.692658234374996518, -28.56770833299193413, 4.663820869356208654 ) ) ;
#4405 = UNCERTAINTY_MEASURE_WITH_UNIT (LENGTH_MEASURE( 1.000000000000000082E-05 ), #6796, 'distance_accuracy_value', 'NONE');
#4406 = CARTESIAN_POINT ( 'NONE',  ( 2.557341765624996821, -27.40104166700806587, 4.429445870380401828 ) ) ;
#4407 = CARTESIAN_POINT ( 'NONE',  ( 0.000000000000000000, -30.00000000000000000, 5.250000000000000000 ) ) ;
#4408 = CARTESIAN_POINT ( 'NONE',  ( 0.000000000000000000, -9.999999999999998224, 0.000000000000000000 ) ) ;
#4409 = CARTESIAN_POINT ( 'NONE',  ( -3.000000000000000444, -2.950659073900639306, 0.01814118441314532468 ) ) ;
#4410 = CARTESIAN_POINT ( 'NONE',  ( -2.625000000000000444, -29.47916666598386826, -4.546633369868303021 ) ) ;
#4411 = CARTESIAN_POINT ( 'NONE',  ( -1.638713065079163034, -3.149340926099360782, -4.007514324621466173 ) ) ;
#4412 = ADVANCED_FACE ( 'NONE', ( #4164 ), #6998, .T. ) ;
#4413 = CARTESIAN_POINT ( 'NONE',  ( 2.625000000000002220, -28.10416666598386826, 4.546633369868302132 ) ) ;
#4414 = CARTESIAN_POINT ( 'NONE',  ( -2.625000000000000444, -27.72916666598386826, -4.546633369868303021 ) ) ;
#4415 = CARTESIAN_POINT ( 'NONE',  ( -2.625000000000002220, -27.83333333333333215, 4.546633369868302132 ) ) ;
#4416 = EDGE_CURVE ( 'NONE', #7256, #6014, #3790, .T. ) ;
#4417 = CARTESIAN_POINT ( 'NONE',  ( 2.625000000000002220, -29.85416666598387181, 4.546633369868302132 ) ) ;
#4418 = EDGE_LOOP ( 'NONE', ( #7417, #3410, #1679, #6191 ) ) ;
#4419 = CARTESIAN_POINT ( 'NONE',  ( -5.385316468750001029, -27.59895833299193413, -3.109213912904136734 ) ) ;
#4420 = DIRECTION ( 'NONE',  ( 1.000000000000000000, 0.000000000000000000, 0.000000000000000000 ) ) ;
#4421 = ORIENTED_EDGE ( 'NONE', *, *, #3950, .T. ) ;
#4422 = CYLINDRICAL_SURFACE ( 'NONE', #5382, 5.250000000000000000 ) ;
#4423 = CARTESIAN_POINT ( 'NONE',  ( -0.01814118441314477650, -4.150659073900639484, -3.000000000000000444 ) ) ;
#4424 = EDGE_LOOP ( 'NONE', ( #1463, #3632, #7619, #5278 ) ) ;
#4425 = CARTESIAN_POINT ( 'NONE',  ( 3.712013335537174572E-16, -29.43750000000000000, -6.062177826491070398 ) ) ;
#4426 = CARTESIAN_POINT ( 'NONE',  ( 2.557341765624996821, -27.71354166700806587, 4.429445870380401828 ) ) ;
#4427 = CARTESIAN_POINT ( 'NONE',  ( 5.250000000000000000, -27.12500000000000000, -6.429395695523604153E-16 ) ) ;
#4428 = CARTESIAN_POINT ( 'NONE',  ( -2.625000000000000444, -29.97916666598387181, -4.546633369868303021 ) ) ;
#4429 = CARTESIAN_POINT ( 'NONE',  ( -3.500000000000000000, -6.649340926099361226, -0.01814118441321344033 ) ) ;
#4430 = CARTESIAN_POINT ( 'NONE',  ( -3.750000000000000000, 0.000000000000000000, -3.927886379372531234E-14 ) ) ;
#4431 = CARTESIAN_POINT ( 'NONE',  ( -5.249999999999999112, -27.42708333401612819, -3.031088913245536975 ) ) ;
#4432 = CARTESIAN_POINT ( 'NONE',  ( 5.114683531249998971, -29.69270833367473017, 2.952963913586936329 ) ) ;
#4433 = SURFACE_SIDE_STYLE ('',( #5824 ) ) ;
#4434 = ORIENTED_EDGE ( 'NONE', *, *, #2572, .F. ) ;
#4435 = DIRECTION ( 'NONE',  ( 0.000000000000000000, 1.000000000000000000, 0.000000000000000000 ) ) ;
#4436 = CARTESIAN_POINT ( 'NONE',  ( -1.975475456537005874E-15, -28.84375000068279959, 5.249999999999999112 ) ) ;
#4437 = CARTESIAN_POINT ( 'NONE',  ( 5.114683531250000748, -28.35937500034139447, 0.000000000000000000 ) ) ;
#4438 = AXIS2_PLACEMENT_3D ( 'NONE', #3216, #6737, #4465 ) ;
#4439 = ORIENTED_EDGE ( 'NONE', *, *, #3553, .T. ) ;
#4440 = DIRECTION ( 'NONE',  ( 0.000000000000000000, 1.000000000000000000, 0.000000000000000000 ) ) ;
#4441 = CARTESIAN_POINT ( 'NONE',  ( 1.142306659890740623E-15, -27.54687499965860198, 6.218427825808274356 ) ) ;
#4442 = CARTESIAN_POINT ( 'NONE',  ( 4.007514324621432422, -6.850659073900641438, 1.638713065079246078 ) ) ;
#4443 = DIRECTION ( 'NONE',  ( -0.000000000000000000, 1.000000000000000000, -0.000000000000000000 ) ) ;
#4444 = ORIENTED_EDGE ( 'NONE', *, *, #8843, .F. ) ;
#4445 = CARTESIAN_POINT ( 'NONE',  ( 1.975475456537005874E-15, -27.93749999999999289, 5.249999999999999112 ) ) ;
#4446 = CARTESIAN_POINT ( 'NONE',  ( 2.625000000000000444, -29.48958333401613174, -4.546633369868303021 ) ) ;
#4447 = CARTESIAN_POINT ( 'NONE',  ( -2.692658234374996518, -28.06770833299193413, 4.663820869356208654 ) ) ;
#4448 = CARTESIAN_POINT ( 'NONE',  ( 3.616337804771879580E-16, -27.54687500034140157, -5.905927827173866440 ) ) ;
#4449 = CARTESIAN_POINT ( 'NONE',  ( 2.300847884672513123E-14, -27.46875000068279604, -5.250000000000000000 ) ) ;
#4450 = CARTESIAN_POINT ( 'NONE',  ( 2.692658234375002735, -27.49479166632526628, 4.663820869356205101 ) ) ;
#4451 = CARTESIAN_POINT ( 'NONE',  ( -2.992485675378538268, -8.149340926099366555, -1.260781871532495879 ) ) ;
#4452 =( GEOMETRIC_REPRESENTATION_CONTEXT ( 3 ) GLOBAL_UNCERTAINTY_ASSIGNED_CONTEXT ( ( #345 ) ) GLOBAL_UNIT_ASSIGNED_CONTEXT ( ( #5708, #8552, #4189 ) ) REPRESENTATION_CONTEXT ( 'NONE', 'WORKASPACE' ) );
#4453 = DIRECTION ( 'NONE',  ( 0.000000000000000000, -1.000000000000000000, 0.000000000000000000 ) ) ;
#4454 = CARTESIAN_POINT ( 'NONE',  ( -1.638713065079163034, -4.749340926099361759, -4.007514324621466173 ) ) ;
#4455 = AXIS2_PLACEMENT_3D ( 'NONE', #314, #8089, #5150 ) ;
#4456 = EDGE_CURVE ( 'NONE', #4617, #2202, #7121, .T. ) ;
#4457 = CARTESIAN_POINT ( 'NONE',  ( 5.250000000000000000, -27.31249999931720396, -6.429395695523604153E-16 ) ) ;
#4458 = CARTESIAN_POINT ( 'NONE',  ( 3.500000000000000000, -2.649340926099361226, 0.01814118441321387054 ) ) ;
#4459 = VECTOR ( 'NONE', #4393, 1000.000000000000000 ) ;
#4460 = EDGE_CURVE ( 'NONE', #3057, #6454, #3544, .T. ) ;
#4461 = CARTESIAN_POINT ( 'NONE',  ( 2.161402558328724325E-14, -29.74999999931720396, -5.250000000000000000 ) ) ;
#4462 = ORIENTED_EDGE ( 'NONE', *, *, #1859, .F. ) ;
#4463 = CARTESIAN_POINT ( 'NONE',  ( -5.385316468750000141, -28.32812499965860198, 0.000000000000000000 ) ) ;
#4464 = CARTESIAN_POINT ( 'NONE',  ( -2.841254879263533262, -6.849340926099361404, 2.815599370228847764 ) ) ;
#4465 = DIRECTION ( 'NONE',  ( 0.000000000000000000, 0.000000000000000000, -1.000000000000000000 ) ) ;
#4466 = ORIENTED_EDGE ( 'NONE', *, *, #3453, .F. ) ;
#4467 = CARTESIAN_POINT ( 'NONE',  ( 2.692658234374998738, -27.16145833299193413, -4.663820869356206877 ) ) ;
#4468 = CARTESIAN_POINT ( 'NONE',  ( 2.487701488670203354, -0.3506590739006389956, 2.462045979635629323 ) ) ;
#4469 = ORIENTED_EDGE ( 'NONE', *, *, #8173, .F. ) ;
#4470 = CARTESIAN_POINT ( 'NONE',  ( -1.113604000661152470E-15, -27.31250000000000000, 6.062177826491070398 ) ) ;
#4471 = EDGE_CURVE ( 'NONE', #4009, #1967, #2563, .T. ) ;
#4472 = CARTESIAN_POINT ( 'NONE',  ( 5.114683531250000748, -27.65104166700806587, -2.952963913586932776 ) ) ;
#4473 = AXIS2_PLACEMENT_3D ( 'NONE', #5332, #1907, #3395 ) ;
#4474 = SURFACE_STYLE_FILL_AREA ( #2478 ) ;
#4475 = DIRECTION ( 'NONE',  ( 0.000000000000000000, -0.000000000000000000, 1.000000000000000000 ) ) ;
#4476 = DIRECTION ( 'NONE',  ( 0.000000000000000000, 0.000000000000000000, 1.000000000000000000 ) ) ;
#4477 = CARTESIAN_POINT ( 'NONE',  ( -1.431606283892620235, -1.549340926099361138, -3.507514324621463953 ) ) ;
#4478 = EDGE_CURVE ( 'NONE', #7180, #4261, #5218, .T. ) ;
#4479 = EDGE_CURVE ( 'NONE', #3341, #5696, #2005, .T. ) ;
#4480 = CARTESIAN_POINT ( 'NONE',  ( -1.406733220335620871, -29.98883544994945538, -5.250000023052310283 ) ) ;
#4481 = CARTESIAN_POINT ( 'NONE',  ( 5.249999999999999112, -28.72916666666666785, -3.031088913245534755 ) ) ;
#4482 = CARTESIAN_POINT ( 'NONE',  ( 5.114683531249999859, -29.40104166700806232, -2.952963913586932776 ) ) ;
#4483 = DIRECTION ( 'NONE',  ( 0.000000000000000000, 0.000000000000000000, -1.000000000000000000 ) ) ;
#4484 = EDGE_LOOP ( 'NONE', ( #6407, #6798, #7135, #4561 ) ) ;
#4485 = EDGE_CURVE ( 'NONE', #3224, #1598, #5915, .T. ) ;
#4486 = CARTESIAN_POINT ( 'NONE',  ( 1.975475456537005874E-15, -28.12499999931720041, 5.250000000000000000 ) ) ;
#4487 = CARTESIAN_POINT ( 'NONE',  ( 6.972266317189433020E-16, -27.93749999999999289, -5.250000000000000000 ) ) ;
#4488 = CARTESIAN_POINT ( 'NONE',  ( -2.557341765624999042, -28.52604166700806587, -4.429445870380400052 ) ) ;
#4489 = EDGE_CURVE ( 'NONE', #3220, #946, #7342, .T. ) ;
#4490 = ORIENTED_EDGE ( 'NONE', *, *, #672, .T. ) ;
#4491 = DIRECTION ( 'NONE',  ( 0.000000000000000000, -1.000000000000000000, 0.000000000000000000 ) ) ;
#4492 = CARTESIAN_POINT ( 'NONE',  ( 5.385316468749999252, -27.71354166632526272, -3.109213912904138954 ) ) ;
#4493 = ADVANCED_FACE ( 'NONE', ( #3092, #7176 ), #5772, .F. ) ;
#4494 = CARTESIAN_POINT ( 'NONE',  ( 1.674995433905515085, -3.450659073900638862, 3.992485675378568022 ) ) ;
#4495 = CARTESIAN_POINT ( 'NONE',  ( -2.625000000000002220, -29.08333333333333215, 4.546633369868302132 ) ) ;
#4496 = VERTEX_POINT ( 'NONE', #5823 ) ;
#4497 =( BOUNDED_CURVE ( )  B_SPLINE_CURVE ( 2, ( #8628, #1655, #4399, #3062, #1602, #5882, #907, #3754, #6580 ),
 .UNSPECIFIED., .F., .F. ) 
 B_SPLINE_CURVE_WITH_KNOTS ( ( 3, 2, 2, 2, 3 ),
 ( 0.8125000000000000000, 0.8194444444444444198, 0.8333333333333333703, 0.8472222222222222099, 0.8541666666666666297 ),
 .UNSPECIFIED. ) 
 CURVE ( )  GEOMETRIC_REPRESENTATION_ITEM ( )  RATIONAL_B_SPLINE_CURVE ( ( 0.9330127018922194093, 0.9330127018922194093, 1.000000000000000000, 0.8660254037844387076, 1.000000000000000000, 0.8660254037844387076, 1.000000000000000000, 0.9330127018922198534, 0.9330127018922192983 ) ) 
 REPRESENTATION_ITEM ( '' )  );
#4498 = CARTESIAN_POINT ( 'NONE',  ( -2.033577675846918216E-14, -29.93750000000000355, 5.250000000000000888 ) ) ;
#4499 = CARTESIAN_POINT ( 'NONE',  ( 2.624999999999996891, -29.07291666734946389, 4.546633369868304797 ) ) ;
#4500 = CARTESIAN_POINT ( 'NONE',  ( -5.385316468749998364, -27.83854166632526628, 3.109213912904140287 ) ) ;
#4501 = CARTESIAN_POINT ( 'NONE',  ( 5.114683531250000748, -27.85937500034139802, 0.000000000000000000 ) ) ;
#4502 = AXIS2_PLACEMENT_3D ( 'NONE', #4977, #7084, #16 ) ;
#4503 = VERTEX_POINT ( 'NONE', #3744 ) ;
#4504 = CARTESIAN_POINT ( 'NONE',  ( -5.385316468750001029, -27.59895833299194123, -3.109213912904136734 ) ) ;
#4505 = CARTESIAN_POINT ( 'NONE',  ( -1.224499502706140497, -1.650659073900639484, 3.007514324621436863 ) ) ;
#4506 = CARTESIAN_POINT ( 'NONE',  ( 0.000000000000000000, -9.999999999999998224, 0.000000000000000000 ) ) ;
#4507 = CARTESIAN_POINT ( 'NONE',  ( 4.007514324621469726, -1.149340926099360782, -1.638713065079161257 ) ) ;
#4508 = AXIS2_PLACEMENT_3D ( 'NONE', #3859, #1714, #5148 ) ;
#4509 = VECTOR ( 'NONE', #5770, 1000.000000000000114 ) ;
#4510 = CARTESIAN_POINT ( 'NONE',  ( -2.624999999999996891, -27.64583333265053611, 4.546633369868304797 ) ) ;
#4511 = CARTESIAN_POINT ( 'NONE',  ( -6.972266317189433020E-16, -27.06250000000000000, -5.250000000000000000 ) ) ;
#4512 = CARTESIAN_POINT ( 'NONE',  ( -2.462045979635576920, -3.249340926099361315, -2.487701488670255756 ) ) ;
#4513 = DIRECTION ( 'NONE',  ( 0.000000000000000000, 0.000000000000000000, 1.000000000000000000 ) ) ;
#4514 = DIRECTION ( 'NONE',  ( 0.000000000000000000, 0.000000000000000000, 1.000000000000000000 ) ) ;
#4515 = CARTESIAN_POINT ( 'NONE',  ( 5.385316468750001029, -27.72395833299193413, 3.109213912904135846 ) ) ;
#4516 = CARTESIAN_POINT ( 'NONE',  ( 4.000000000000000000, -5.849340926099360516, 0.01814118441321914063 ) ) ;
#4517 = AXIS2_PLACEMENT_3D ( 'NONE', #4198, #1312, #7166 ) ;
#4518 = DIRECTION ( 'NONE',  ( 0.000000000000000000, 0.000000000000000000, 1.000000000000000000 ) ) ;
#4519 = ORIENTED_EDGE ( 'NONE', *, *, #4478, .F. ) ;
#4520 = CARTESIAN_POINT ( 'NONE',  ( -5.385316468750001029, -28.84895833299193413, -3.109213912904136734 ) ) ;
#4521 = CARTESIAN_POINT ( 'NONE',  ( -3.000000000000000444, -4.550659073900638951, 0.01814118441314532468 ) ) ;
#4522 = EDGE_LOOP ( 'NONE', ( #1355, #7638, #523, #8955 ) ) ;
#4523 = CARTESIAN_POINT ( 'NONE',  ( 5.250000000000000000, -28.24999999999999645, 0.000000000000000000 ) ) ;
#4524 = EDGE_CURVE ( 'NONE', #4744, #7091, #4930, .T. ) ;
#4525 = CARTESIAN_POINT ( 'NONE',  ( 3.492485675378566690, -3.850659073900639218, -1.467888652718972287 ) ) ;
#4526 = CARTESIAN_POINT ( 'NONE',  ( 5.250000000000000000, -27.62500000000000000, -6.429395695523604153E-16 ) ) ;
#4527 = CARTESIAN_POINT ( 'NONE',  ( 5.250000000000000888, -30.08333333265053255, 3.031088913245532979 ) ) ;
#4528 = CARTESIAN_POINT ( 'NONE',  ( 3.500000000000000000, -1.049340926099360916, 0.01814118441321387054 ) ) ;
#4529 = CARTESIAN_POINT ( 'NONE',  ( 2.624999999999996891, -28.82291666734946389, 4.546633369868304797 ) ) ;
#4530 = CARTESIAN_POINT ( 'NONE',  ( -1.000000000000000000, -32.99989163573538775, 2.732192776429915426 ) ) ;
#4531 = CARTESIAN_POINT ( 'NONE',  ( -5.114683531249999859, -28.56770833367473017, -2.952963913586935440 ) ) ;
#4532 = CARTESIAN_POINT ( 'NONE',  ( 2.625000000000000444, -28.23958333401612819, -4.546633369868303021 ) ) ;
#4533 = EDGE_LOOP ( 'NONE', ( #762, #5883, #6020, #7756 ) ) ;
#4534 = DIRECTION ( 'NONE',  ( 0.000000000000000000, 0.000000000000000000, -1.000000000000000000 ) ) ;
#4535 = CARTESIAN_POINT ( 'NONE',  ( 2.557341765625000818, -28.56770833367473017, -4.429445870380400052 ) ) ;
#4536 = ORIENTED_EDGE ( 'NONE', *, *, #3417, .T. ) ;
#4537 = CARTESIAN_POINT ( 'NONE',  ( -5.385316468749998364, -27.58854166632526628, 3.109213912904140287 ) ) ;
#4538 = CARTESIAN_POINT ( 'NONE',  ( 2.815599370228907716, -7.150659073900638596, -2.841254879263473310 ) ) ;
#4539 = UNCERTAINTY_MEASURE_WITH_UNIT (LENGTH_MEASURE( 1.000000000000000082E-05 ), #4046, 'distance_accuracy_value', 'NONE');
#4540 = CARTESIAN_POINT ( 'NONE',  ( -6.972266317189433020E-16, -29.24999999931720396, -5.250000000000000000 ) ) ;
#4541 = CARTESIAN_POINT ( 'NONE',  ( -5.385316468750001029, -28.13020833299193058, -3.109213912904136734 ) ) ;
#4542 = ORIENTED_EDGE ( 'NONE', *, *, #3950, .F. ) ;
#4543 = CARTESIAN_POINT ( 'NONE',  ( 2.625000000000002220, -29.91666666666666785, 4.546633369868302132 ) ) ;
#4544 = CARTESIAN_POINT ( 'NONE',  ( -2.624999999999998668, -28.69791666734946389, -4.546633369868303021 ) ) ;
#4545 = CARTESIAN_POINT ( 'NONE',  ( 5.385316468749999252, -27.46354166632526983, -3.109213912904139399 ) ) ;
#4546 = CARTESIAN_POINT ( 'NONE',  ( 5.114683531249998971, -27.13020833367473372, 2.952963913586936329 ) ) ;
#4547 = VERTEX_POINT ( 'NONE', #3974 ) ;
#4548 = CARTESIAN_POINT ( 'NONE',  ( 0.000000000000000000, 69.99999999999998579, 0.000000000000000000 ) ) ;
#4549 = CARTESIAN_POINT ( 'NONE',  ( -2.134148098076932953, -2.750659073900639573, -2.108492589042352705 ) ) ;
#4550 = FACE_OUTER_BOUND ( 'NONE', #5562, .T. ) ;
#4551 = SHAPE_REPRESENTATION ( 'outer body', ( #888 ), #6342 ) ;
#4552 = CARTESIAN_POINT ( 'NONE',  ( 5.250000000000000888, -27.83333333265053611, 3.031088913245532979 ) ) ;
#4553 = CARTESIAN_POINT ( 'NONE',  ( 0.000000000000000000, -46.00000000000000000, -2.999999999999999556 ) ) ;
#4554 = CARTESIAN_POINT ( 'NONE',  ( -0.01814118441321365544, -3.849340926099361404, 3.500000000000000000 ) ) ;
#4555 = CARTESIAN_POINT ( 'NONE',  ( -2.033577675846918216E-14, -29.18750000000000000, 5.250000000000000888 ) ) ;
#4556 = ORIENTED_EDGE ( 'NONE', *, *, #6707, .F. ) ;
#4557 = CARTESIAN_POINT ( 'NONE',  ( 2.692658234375002735, -28.49479166632526628, 4.663820869356205101 ) ) ;
#4558 = EDGE_CURVE ( 'NONE', #3585, #7800, #8296, .T. ) ;
#4559 = CARTESIAN_POINT ( 'NONE',  ( -1.638713065079163034, -1.549340926099360916, -4.007514324621466173 ) ) ;
#4560 = CARTESIAN_POINT ( 'NONE',  ( -5.250000000000000888, -29.60416666666666430, 3.031088913245533423 ) ) ;
#4561 = ORIENTED_EDGE ( 'NONE', *, *, #2021, .T. ) ;
#4562 = CARTESIAN_POINT ( 'NONE',  ( -5.385316468750000141, -28.32812499965860198, 0.000000000000000000 ) ) ;
#4563 = CARTESIAN_POINT ( 'NONE',  ( 3.000000000000000444, -3.750659073900639573, -0.01814118441314496039 ) ) ;
#4564 = ORIENTED_EDGE ( 'NONE', *, *, #5081, .F. ) ;
#4565 = CARTESIAN_POINT ( 'NONE',  ( 2.624999999999996891, -28.29166666666666785, 4.546633369868304797 ) ) ;
#4566 = CARTESIAN_POINT ( 'NONE',  ( -2.487701488670202910, -2.750659073900639129, -2.462045979635629767 ) ) ;
#4567 = PRESENTATION_LAYER_ASSIGNMENT (  '', '', ( #9162 ) ) ;
#4568 = VERTEX_POINT ( 'NONE', #1835 ) ;
#4569 = CARTESIAN_POINT ( 'NONE',  ( -5.250000000000000000, -29.40625000068279604, -6.429395695523604153E-16 ) ) ;
#4570 = ORIENTED_EDGE ( 'NONE', *, *, #933, .T. ) ;
#4571 = CARTESIAN_POINT ( 'NONE',  ( -2.557341765624999042, -29.52604166700806232, -4.429445870380400052 ) ) ;
#4572 = CARTESIAN_POINT ( 'NONE',  ( -2.462045979635576920, -4.849340926099361404, -2.487701488670255756 ) ) ;
#4573 = CARTESIAN_POINT ( 'NONE',  ( 1.406733260263403507, -29.51116454900182973, -5.249999999999994671 ) ) ;
#4574 = CARTESIAN_POINT ( 'NONE',  ( -5.250000000000000000, -28.12499999999999645, -6.429395695523604153E-16 ) ) ;
#4575 = CARTESIAN_POINT ( 'NONE',  ( -2.557341765625002594, -29.00520833367473017, 4.429445870380399164 ) ) ;
#4576 = STYLED_ITEM ( 'NONE', ( #4964 ), #7073 ) ;
#4577 = FACE_OUTER_BOUND ( 'NONE', #757, .T. ) ;
#4578 = ORIENTED_EDGE ( 'NONE', *, *, #8719, .F. ) ;
#4579 = CARTESIAN_POINT ( 'NONE',  ( -5.250000000000000888, -27.88541666734946389, 3.031088913245533423 ) ) ;
#4580 = CARTESIAN_POINT ( 'NONE',  ( -2.557341765625002594, -27.19270833367473017, 4.429445870380399164 ) ) ;
#4581 = ORIENTED_EDGE ( 'NONE', *, *, #6056, .F. ) ;
#4582 = CARTESIAN_POINT ( 'NONE',  ( 2.300847884672513123E-14, -27.43750000000000355, -5.250000000000000000 ) ) ;
#4583 = CARTESIAN_POINT ( 'NONE',  ( -3.807688866302469071E-16, -28.92187499965859487, -6.218427825808274356 ) ) ;
#4584 = CARTESIAN_POINT ( 'NONE',  ( 2.815599370228907716, -3.950659073900640195, -2.841254879263473310 ) ) ;
#4585 = FILL_AREA_STYLE_COLOUR ( '', #5334 ) ;
#4586 = CARTESIAN_POINT ( 'NONE',  ( -5.385316468749998364, -28.08854166632526628, 3.109213912904140287 ) ) ;
#4587 = ORIENTED_EDGE ( 'NONE', *, *, #6878, .F. ) ;
#4588 = ADVANCED_FACE ( 'NONE', ( #478 ), #3324, .T. ) ;
#4589 = DIRECTION ( 'NONE',  ( 0.000000000000000000, 0.000000000000000000, -1.000000000000000000 ) ) ;
#4590 = CARTESIAN_POINT ( 'NONE',  ( -5.250000000000000000, -27.67708333401612464, -3.031088913245536531 ) ) ;
#4591 = CARTESIAN_POINT ( 'NONE',  ( -2.692658234375000514, -27.40104166632526628, -4.663820869356205989 ) ) ;
#4592 = ORIENTED_EDGE ( 'NONE', *, *, #2304, .F. ) ;
#4593 = CONICAL_SURFACE ( 'NONE', #586, 5.257453848358681014, 0.1221730476396033355 ) ;
#4594 = CARTESIAN_POINT ( 'NONE',  ( -5.385316468750001029, -28.34895833299193413, -3.109213912904136734 ) ) ;
#4595 = CARTESIAN_POINT ( 'NONE',  ( -0.01814118441314477650, -4.150659073900639484, -3.000000000000000444 ) ) ;
#4596 = CARTESIAN_POINT ( 'NONE',  ( 2.324088772396477476E-15, -27.49999999931720751, -5.250000000000000000 ) ) ;
#4597 = PRODUCT ( 'outer body', 'outer body', '', ( #3400 ) ) ;
#4598 = CARTESIAN_POINT ( 'NONE',  ( 5.250000000000000888, -28.33333333265053611, 3.031088913245532979 ) ) ;
#4599 = CARTESIAN_POINT ( 'NONE',  ( -2.624999999999996891, -27.64583333265053611, 4.546633369868304797 ) ) ;
#4600 = CARTESIAN_POINT ( 'NONE',  ( 1.467888652719048226, -2.949340926099361049, -3.492485675378535603 ) ) ;
#4601 = CARTESIAN_POINT ( 'NONE',  ( 2.625000000000000444, -29.70833333333333215, -4.546633369868303021 ) ) ;
#4602 = ORIENTED_EDGE ( 'NONE', *, *, #5006, .T. ) ;
#4603 = CARTESIAN_POINT ( 'NONE',  ( 0.000000000000000000, 0.000000000000000000, 0.000000000000000000 ) ) ;
#4604 = CARTESIAN_POINT ( 'NONE',  ( 5.385316468750001029, -27.97395833299193413, 3.109213912904135846 ) ) ;
#4605 = CARTESIAN_POINT ( 'NONE',  ( 0.01814118441321938349, -7.849340926099360516, -4.000000000000000000 ) ) ;
#4606 = DIRECTION ( 'NONE',  ( 0.000000000000000000, 0.000000000000000000, 1.000000000000000000 ) ) ;
#4607 = VERTEX_POINT ( 'NONE', #6052 ) ;
#4608 = CIRCLE ( 'NONE', #4155, 0.2499999999999998335 ) ;
#4609 = CARTESIAN_POINT ( 'NONE',  ( -5.385316468750001029, -28.09895833299193413, -3.109213912904136734 ) ) ;
#4610 = CARTESIAN_POINT ( 'NONE',  ( -2.462045979635629323, -1.550659073900639173, 2.487701488670203798 ) ) ;
#4611 = ORIENTED_EDGE ( 'NONE', *, *, #867, .T. ) ;
#4612 = CARTESIAN_POINT ( 'NONE',  ( -2.624999999999998668, -27.91666666666666430, -4.546633369868303021 ) ) ;
#4613 = CARTESIAN_POINT ( 'NONE',  ( 2.462045979635629767, -0.7506590739006389068, -2.487701488670203354 ) ) ;
#4614 = VERTEX_POINT ( 'NONE', #1033 ) ;
#4615 = CARTESIAN_POINT ( 'NONE',  ( 5.114683531250000748, -26.92187500034139802, 0.000000000000000000 ) ) ;
#4616 = AXIS2_PLACEMENT_3D ( 'NONE', #1525, #733, #7065 ) ;
#4617 = VERTEX_POINT ( 'NONE', #5451 ) ;
#4618 = CARTESIAN_POINT ( 'NONE',  ( -5.114683531250001636, -28.96354166700807298, 2.952963913586931444 ) ) ;
#4619 = CARTESIAN_POINT ( 'NONE',  ( -2.134148098076978251, -0.4493409260993615484, 2.108492589042307408 ) ) ;
#4620 = CARTESIAN_POINT ( 'NONE',  ( 6.972266317189434006E-16, -27.24999999931720751, -5.250000000000000000 ) ) ;
#4621 = CARTESIAN_POINT ( 'NONE',  ( 0.000000000000000000, 69.99999999999998579, 0.000000000000000000 ) ) ;
#4622 = CARTESIAN_POINT ( 'NONE',  ( -2.557341765624999042, -28.08854166700806587, -4.429445870380400052 ) ) ;
#4623 = DIRECTION ( 'NONE',  ( 0.000000000000000000, -1.000000000000000000, 0.000000000000000000 ) ) ;
#4624 = CARTESIAN_POINT ( 'NONE',  ( -5.114683531249999859, -27.50520833367472662, -2.952963913586935440 ) ) ;
#4625 = ORIENTED_EDGE ( 'NONE', *, *, #7129, .T. ) ;
#4626 =( BOUNDED_CURVE ( )  B_SPLINE_CURVE ( 2, ( #2115, #6428, #2825, #20, #5688, #8533, #4940, #9091, #64 ),
 .UNSPECIFIED., .F., .F. ) 
 B_SPLINE_CURVE_WITH_KNOTS ( ( 3, 2, 2, 2, 3 ),
 ( 0.5625000000000000000, 0.5694444444444444198, 0.5833333333333333703, 0.5972222222222222099, 0.6041666666666667407 ),
 .UNSPECIFIED. ) 
 CURVE ( )  GEOMETRIC_REPRESENTATION_ITEM ( )  RATIONAL_B_SPLINE_CURVE ( ( 0.9330127018922194093, 0.9330127018922194093, 1.000000000000000000, 0.8660254037844387076, 1.000000000000000000, 0.8660254037844387076, 1.000000000000000000, 0.9330127018922187432, 0.9330127018922192983 ) ) 
 REPRESENTATION_ITEM ( '' )  );
#4627 = DIRECTION ( 'NONE',  ( 0.000000000000000000, 0.000000000000000000, -1.000000000000000000 ) ) ;
#4628 = EDGE_CURVE ( 'NONE', #849, #4614, #2632, .T. ) ;
#4629 = CARTESIAN_POINT ( 'NONE',  ( 5.385316468750001029, -28.50520833299193058, 3.109213912904134958 ) ) ;
#4630 = CARTESIAN_POINT ( 'NONE',  ( -1.975475456537005874E-15, -29.09375000068278894, 5.250000000000000000 ) ) ;
#4631 = DIRECTION ( 'NONE',  ( 0.000000000000000000, 1.000000000000000000, 0.000000000000000000 ) ) ;
#4632 = CARTESIAN_POINT ( 'NONE',  ( -2.692658234375000514, -29.40104166632526983, -4.663820869356205989 ) ) ;
#4633 = ORIENTED_EDGE ( 'NONE', *, *, #3740, .F. ) ;
#4634 = CARTESIAN_POINT ( 'NONE',  ( -6.972266317189433020E-16, -28.31249999999999645, -5.250000000000000000 ) ) ;
#4635 = CARTESIAN_POINT ( 'NONE',  ( 3.712013335537174572E-16, -27.46875000068279959, -6.062177826491070398 ) ) ;
#4636 = CARTESIAN_POINT ( 'NONE',  ( 2.692658234375002735, -29.27604166632526983, 4.663820869356205101 ) ) ;
#4637 = ADVANCED_FACE ( 'NONE', ( #4667 ), #4757, .T. ) ;
#4638 = ORIENTED_EDGE ( 'NONE', *, *, #1077, .T. ) ;
#4639 = CARTESIAN_POINT ( 'NONE',  ( 5.385316468749999252, -27.68229166632526272, -3.109213912904138954 ) ) ;
#4640 = CARTESIAN_POINT ( 'NONE',  ( 3.500000000000000000, -2.150659073900639040, -0.01814118441313969030 ) ) ;
#4641 = ADVANCED_BREP_SHAPE_REPRESENTATION ( '', ( #2131, #888 ), #6342 ) ;
#4642 = DIRECTION ( 'NONE',  ( 0.000000000000000000, 1.000000000000000000, 0.000000000000000000 ) ) ;
#4643 = CARTESIAN_POINT ( 'NONE',  ( 0.000000000000000000, -46.00000000000000000, 0.000000000000000000 ) ) ;
#4644 = CARTESIAN_POINT ( 'NONE',  ( 2.462045979635577364, -2.449340926099361049, 2.487701488670255312 ) ) ;
#4645 = VECTOR ( 'NONE', #239, 1000.000000000000000 ) ;
#4646 = CARTESIAN_POINT ( 'NONE',  ( 5.114683531249999859, -29.58854166700806232, -2.952963913586932776 ) ) ;
#4647 = CARTESIAN_POINT ( 'NONE',  ( 5.249999999999997335, -27.77083333333333215, 3.031088913245538308 ) ) ;
#4648 = PRODUCT_CONTEXT ( 'NONE', #8005, 'mechanical' ) ;
#4649 = CARTESIAN_POINT ( 'NONE',  ( -5.385316468750001029, -29.84895833299193413, -3.109213912904136734 ) ) ;
#4650 = CARTESIAN_POINT ( 'NONE',  ( -1.260781871532494103, -0.5493409260993613596, 2.992485675378538712 ) ) ;
#4651 = CARTESIAN_POINT ( 'NONE',  ( 5.385316468750001029, -27.72395833299193413, 3.109213912904135846 ) ) ;
#4652 = CARTESIAN_POINT ( 'NONE',  ( 1.431606283892694842, -2.450659073900638862, -3.507514324621434199 ) ) ;
#4653 = VERTEX_POINT ( 'NONE', #6855 ) ;
#4654 = CARTESIAN_POINT ( 'NONE',  ( 5.249999999999999112, -27.77083333333333215, 3.031088913245538308 ) ) ;
#4655 = DIRECTION ( 'NONE',  ( 0.000000000000000000, 1.000000000000000000, 0.000000000000000000 ) ) ;
#4656 = CARTESIAN_POINT ( 'NONE',  ( 5.114683531250000748, -27.15104166700806587, -2.952963913586932776 ) ) ;
#4657 = ADVANCED_FACE ( 'NONE', ( #2484 ), #6104, .T. ) ;
#4658 = AXIS2_PLACEMENT_3D ( 'NONE', #8527, #4934, #6293 ) ;
#4659 = ADVANCED_FACE ( 'NONE', ( #3369 ), #3275, .F. ) ;
#4660 = EDGE_LOOP ( 'NONE', ( #4753, #4816 ) ) ;
#4661 =( LENGTH_UNIT ( ) NAMED_UNIT ( * ) SI_UNIT ( .MILLI., .METRE. ) );
#4662 = CARTESIAN_POINT ( 'NONE',  ( 5.250000000000000000, -28.62500000000000000, -6.429395695523604153E-16 ) ) ;
#4663 = VERTEX_POINT ( 'NONE', #3928 ) ;
#4664 = CARTESIAN_POINT ( 'NONE',  ( -2.557341765624999042, -29.02604166700806587, -4.429445870380400052 ) ) ;
#4665 = CARTESIAN_POINT ( 'NONE',  ( -2.992485675378538268, -1.749340926099361981, -1.260781871532495879 ) ) ;
#4666 = PLANE ( 'NONE',  #5776 ) ;
#4667 = FACE_OUTER_BOUND ( 'NONE', #7053, .T. ) ;
#4668 = CARTESIAN_POINT ( 'NONE',  ( 5.114683531250000748, -28.42187500034139802, 0.000000000000000000 ) ) ;
#4669 = DIRECTION ( 'NONE',  ( 0.000000000000000000, -0.000000000000000000, -1.000000000000000000 ) ) ;
#4670 = DIRECTION ( 'NONE',  ( 0.000000000000000000, -1.000000000000000000, 0.000000000000000000 ) ) ;
#4671 = CARTESIAN_POINT ( 'NONE',  ( 2.557341765624996821, -26.90104166700806232, 4.429445870380401828 ) ) ;
#4672 = PRODUCT_DEFINITION_SHAPE ( 'NONE', 'NONE',  #3486 ) ;
#4673 = ORIENTED_EDGE ( 'NONE', *, *, #1735, .T. ) ;
#4674 = DIRECTION ( 'NONE',  ( -0.000000000000000000, -1.000000000000000000, -0.000000000000000000 ) ) ;
#4675 = CARTESIAN_POINT ( 'NONE',  ( 5.385316468750001029, -29.00520833299193413, 3.109213912904134958 ) ) ;
#4676 = CARTESIAN_POINT ( 'NONE',  ( -2.625000000000002220, -28.58333333333333215, 4.546633369868302132 ) ) ;
#4677 = DIRECTION ( 'NONE',  ( 0.000000000000000000, -1.000000000000000000, 0.000000000000000000 ) ) ;
#4678 = CARTESIAN_POINT ( 'NONE',  ( -3.807688866302469071E-16, -28.92187499965860198, -6.218427825808274356 ) ) ;
#4679 = CARTESIAN_POINT ( 'NONE',  ( -4.000000000000000000, -5.049340926099361582, -0.01814118441321865144 ) ) ;
#4680 = VERTEX_POINT ( 'NONE', #7459 ) ;
#4681 = CYLINDRICAL_SURFACE ( 'NONE', #886, 1.500000000000000222 ) ;
#4682 = CARTESIAN_POINT ( 'NONE',  ( 2.625000000000000444, -27.98958333401612819, -4.546633369868303021 ) ) ;
#4683 = CARTESIAN_POINT ( 'NONE',  ( 1.142306659890740623E-15, -29.04687499965859843, 6.218427825808274356 ) ) ;
#4684 = ORIENTED_EDGE ( 'NONE', *, *, #2568, .F. ) ;
#4685 = CARTESIAN_POINT ( 'NONE',  ( 2.692658234374998738, -28.16145833299193413, -4.663820869356206877 ) ) ;
#4686 = CARTESIAN_POINT ( 'NONE',  ( 2.992485675378565357, -7.050659073900639839, -1.260781871532430376 ) ) ;
#4687 = CARTESIAN_POINT ( 'NONE',  ( 0.000000000000000000, -53.00000000000000000, 0.000000000000000000 ) ) ;
#4688 = ADVANCED_FACE ( 'NONE', ( #3187 ), #7506, .T. ) ;
#4689 = CARTESIAN_POINT ( 'NONE',  ( 5.250000000000000000, -28.24999999999999645, 0.000000000000000000 ) ) ;
#4690 = CARTESIAN_POINT ( 'NONE',  ( 0.000000000000000000, -47.00000000000000000, 0.000000000000000000 ) ) ;
#4691 = CARTESIAN_POINT ( 'NONE',  ( 0.000000000000000000, -20.00000000000000000, 0.000000000000000000 ) ) ;
#4692 = DIRECTION ( 'NONE',  ( 0.000000000000000000, 1.000000000000000000, 0.000000000000000000 ) ) ;
#4693 = SHAPE_DEFINITION_REPRESENTATION ( #7231, #3797 ) ;
#4694 = CARTESIAN_POINT ( 'NONE',  ( 5.385316468750000141, -28.95312499965860198, -6.595110575850215044E-16 ) ) ;
#4695 = CARTESIAN_POINT ( 'NONE',  ( 2.992485675378538712, -0.9493409260993616039, 1.260781871532494103 ) ) ;
#4696 = DIRECTION ( 'NONE',  ( 0.000000000000000000, 0.000000000000000000, -1.000000000000000000 ) ) ;
#4697 = CARTESIAN_POINT ( 'NONE',  ( -5.385316468750000141, -28.82812499965860198, 0.000000000000000000 ) ) ;
#4698 = EDGE_CURVE ( 'NONE', #1434, #3606, #2731, .T. ) ;
#4699 = CARTESIAN_POINT ( 'NONE',  ( 3.507514324621434199, -5.250659073900640905, 1.431606283892693066 ) ) ;
#4700 = ORIENTED_EDGE ( 'NONE', *, *, #2025, .F. ) ;
#4701 = CARTESIAN_POINT ( 'NONE',  ( 2.624999999999996891, -29.04166666666666785, 4.546633369868304797 ) ) ;
#4702 = PLANE ( 'NONE',  #302 ) ;
#4703 = EDGE_CURVE ( 'NONE', #8050, #4395, #8219, .T. ) ;
#4704 = CARTESIAN_POINT ( 'NONE',  ( -1.467888652718973841, -2.650659073900639040, -3.492485675378565801 ) ) ;
#4705 = ORIENTED_EDGE ( 'NONE', *, *, #4754, .F. ) ;
#4706 = FILL_AREA_STYLE_COLOUR ( '', #7840 ) ;
#4707 = CARTESIAN_POINT ( 'NONE',  ( -3.712013335537174572E-16, -29.06250000000000000, -6.062177826491070398 ) ) ;
#4708 = ORIENTED_EDGE ( 'NONE', *, *, #8041, .F. ) ;
#4709 = CARTESIAN_POINT ( 'NONE',  ( -2.557341765625002594, -28.69270833367473017, 4.429445870380399164 ) ) ;
#4710 = CARTESIAN_POINT ( 'NONE',  ( 2.108492589042307408, -2.449340926099361937, 2.134148098076978251 ) ) ;
#4711 = DIRECTION ( 'NONE',  ( 0.000000000000000000, -1.000000000000000000, 0.000000000000000000 ) ) ;
#4712 = CARTESIAN_POINT ( 'NONE',  ( 5.114683531249998971, -27.69270833367472662, 2.952963913586936329 ) ) ;
#4713 = CYLINDRICAL_SURFACE ( 'NONE', #9112, 5.250000000000000000 ) ;
#4714 = FACE_OUTER_BOUND ( 'NONE', #3699, .T. ) ;
#4715 = CARTESIAN_POINT ( 'NONE',  ( 5.114683531250000748, -27.10937500034139802, 0.000000000000000000 ) ) ;
#4716 = CARTESIAN_POINT ( 'NONE',  ( -5.114683531250000748, -29.04687500034139802, -6.263680815196995234E-16 ) ) ;
#4717 =( GEOMETRIC_REPRESENTATION_CONTEXT ( 3 ) GLOBAL_UNCERTAINTY_ASSIGNED_CONTEXT ( ( #2264 ) ) GLOBAL_UNIT_ASSIGNED_CONTEXT ( ( #1781, #5958, #7311 ) ) REPRESENTATION_CONTEXT ( 'NONE', 'WORKASPACE' ) );
#4718 = DIRECTION ( 'NONE',  ( 0.000000000000000000, 0.000000000000000000, 1.000000000000000000 ) ) ;
#4719 = CARTESIAN_POINT ( 'NONE',  ( 5.385316468749999252, -28.46354166632526628, -3.109213912904138954 ) ) ;
#4720 = CARTESIAN_POINT ( 'NONE',  ( -5.249999999999999112, -29.17708333401613174, -3.031088913245536975 ) ) ;
#4721 = LINE ( 'NONE', #7562, #732 ) ;
#4722 = CARTESIAN_POINT ( 'NONE',  ( 5.385316468749999252, -29.46354166632526983, -3.109213912904139399 ) ) ;
#4723 = CARTESIAN_POINT ( 'NONE',  ( -2.841254879263533262, -6.849340926099361404, 2.815599370228847764 ) ) ;
#4724 = ORIENTED_EDGE ( 'NONE', *, *, #5158, .F. ) ;
#4725 = DIRECTION ( 'NONE',  ( 0.000000000000000000, 0.000000000000000000, 1.000000000000000000 ) ) ;
#4726 = CARTESIAN_POINT ( 'NONE',  ( -5.250000000000000888, -27.38541666734946389, 3.031088913245532979 ) ) ;
#4727 = AXIS2_PLACEMENT_3D ( 'NONE', #6686, #2466, #316 ) ;
#4728 = CARTESIAN_POINT ( 'NONE',  ( 5.385316468749999252, -29.71354166632526983, -3.109213912904139399 ) ) ;
#4729 = ORIENTED_EDGE ( 'NONE', *, *, #362, .F. ) ;
#4730 = CARTESIAN_POINT ( 'NONE',  ( 1.142306659890740623E-15, -28.01562499965859843, 6.218427825808274356 ) ) ;
#4731 = CARTESIAN_POINT ( 'NONE',  ( 3.507514324621434199, -2.050659073900638951, 1.431606283892693066 ) ) ;
#4732 = CARTESIAN_POINT ( 'NONE',  ( -6.972266317189433020E-16, -28.31249999999999645, -5.249999999999999112 ) ) ;
#4733 = CARTESIAN_POINT ( 'NONE',  ( 0.000000000000000000, 75.00000000000000000, 5.250000000000000000 ) ) ;
#4734 = DIRECTION ( 'NONE',  ( 0.000000000000000000, 0.000000000000000000, 1.000000000000000000 ) ) ;
#4735 = AXIS2_PLACEMENT_3D ( 'NONE', #2679, #2986, #702 ) ;
#4736 = CARTESIAN_POINT ( 'NONE',  ( -2.557341765624999042, -29.77604166700806232, -4.429445870380400052 ) ) ;
#4737 = ORIENTED_EDGE ( 'NONE', *, *, #191, .T. ) ;
#4738 = CARTESIAN_POINT ( 'NONE',  ( 5.385316468750001029, -29.47395833299193413, 3.109213912904135846 ) ) ;
#4739 = CARTESIAN_POINT ( 'NONE',  ( 2.462045979635577364, -5.649340926099361226, 2.487701488670255312 ) ) ;
#4740 = CARTESIAN_POINT ( 'NONE',  ( 1.406733260263390628, -28.61383544963257108, 5.250000000000001776 ) ) ;
#4741 = CARTESIAN_POINT ( 'NONE',  ( -5.385316468749998364, -29.05729166632526628, 3.109213912904140287 ) ) ;
#4742 = CARTESIAN_POINT ( 'NONE',  ( 1.431606283892694842, -4.050659073900638951, -3.507514324621434199 ) ) ;
#4743 = EDGE_CURVE ( 'NONE', #296, #6874, #7917, .T. ) ;
#4744 = VERTEX_POINT ( 'NONE', #8159 ) ;
#4745 = CARTESIAN_POINT ( 'NONE',  ( -1.406733260263382856, -27.20758545099817027, -5.250000000000006217 ) ) ;
#4746 = AXIS2_PLACEMENT_3D ( 'NONE', #4687, #6027, #8864 ) ;
#4747 = CARTESIAN_POINT ( 'NONE',  ( 0.000000000000000000, -29.00000000000000355, 0.000000000000000000 ) ) ;
#4748 = EDGE_CURVE ( 'NONE', #7800, #1439, #5077, .T. ) ;
#4749 = CARTESIAN_POINT ( 'NONE',  ( -1.431606283892693066, -4.850659073900639662, 3.507514324621434199 ) ) ;
#4750 = ORIENTED_EDGE ( 'NONE', *, *, #4743, .F. ) ;
#4751 = CIRCLE ( 'NONE', #3128, 1.499999999999999778 ) ;
#4752 = CARTESIAN_POINT ( 'NONE',  ( -2.624999999999996891, -28.70833333333333215, 4.546633369868304797 ) ) ;
#4753 = ORIENTED_EDGE ( 'NONE', *, *, #7099, .F. ) ;
#4754 = EDGE_CURVE ( 'NONE', #8128, #946, #427, .T. ) ;
#4755 = CARTESIAN_POINT ( 'NONE',  ( -1.084901341431563726E-15, -29.17187500034139802, 5.905927827173866440 ) ) ;
#4756 = CARTESIAN_POINT ( 'NONE',  ( 3.007514324621463508, -1.149340926099361448, -1.224499502706076770 ) ) ;
#4757 = CYLINDRICAL_SURFACE ( 'NONE', #930, 5.250000000000000000 ) ;
#4758 = CARTESIAN_POINT ( 'NONE',  ( 5.114683531249998971, -27.94270833367473017, 2.952963913586936329 ) ) ;
#4759 = DIRECTION ( 'NONE',  ( 0.000000000000000000, 1.000000000000000000, 0.000000000000000000 ) ) ;
#4760 = CARTESIAN_POINT ( 'NONE',  ( -5.114683531250000748, -27.48437500034139802, -6.263680815196995234E-16 ) ) ;
#4761 = VECTOR ( 'NONE', #5865, 1000.000000000000227 ) ;
#4762 = DIRECTION ( 'NONE',  ( 0.000000000000000000, 1.000000000000000000, 0.000000000000000000 ) ) ;
#4763 = CARTESIAN_POINT ( 'NONE',  ( -2.557341765624999042, -28.83854166700806587, -4.429445870380400052 ) ) ;
#4764 = CARTESIAN_POINT ( 'NONE',  ( 0.000000000000000000, 0.000000000000000000, 0.000000000000000000 ) ) ;
#4765 = CARTESIAN_POINT ( 'NONE',  ( 5.385316468749999252, -28.71354166632526272, -3.109213912904138954 ) ) ;
#4766 = FACE_OUTER_BOUND ( 'NONE', #8557, .T. ) ;
#4767 = CARTESIAN_POINT ( 'NONE',  ( 6.972266317189433020E-16, -29.93750000000000000, -5.250000000000000000 ) ) ;
#4768 = CARTESIAN_POINT ( 'NONE',  ( -2.692658234374996518, -29.06770833299193413, 4.663820869356208654 ) ) ;
#4769 = CARTESIAN_POINT ( 'NONE',  ( -2.487701488670255312, -0.4493409260993610488, 2.462045979635577808 ) ) ;
#4770 = CARTESIAN_POINT ( 'NONE',  ( -1.674995433905599462, -5.349340926099361404, 3.992485675378533383 ) ) ;
#4771 = ORIENTED_EDGE ( 'NONE', *, *, #3446, .T. ) ;
#4772 = CARTESIAN_POINT ( 'NONE',  ( 1.406733260263393293, -28.32366454968462932, -5.250000000000000000 ) ) ;
#4773 = CARTESIAN_POINT ( 'NONE',  ( 5.249999999999999112, -27.80208333401612819, 3.031088913245538308 ) ) ;
#4774 = EDGE_CURVE ( 'NONE', #8385, #8796, #6941, .T. ) ;
#4775 = CARTESIAN_POINT ( 'NONE',  ( -3.807688866302469071E-16, -28.92187499965860198, -6.218427825808274356 ) ) ;
#4776 = EDGE_CURVE ( 'NONE', #1752, #5957, #1971, .T. ) ;
#4777 = ORIENTED_EDGE ( 'NONE', *, *, #756, .F. ) ;
#4778 = CARTESIAN_POINT ( 'NONE',  ( -2.692658234375000514, -28.11979166632526628, -4.663820869356205989 ) ) ;
#4779 = CARTESIAN_POINT ( 'NONE',  ( -3.007514324621435531, -6.050659073900639839, -1.224499502706142273 ) ) ;
#4780 = CARTESIAN_POINT ( 'NONE',  ( 1.000000000000000000, -29.00000000000000355, -1.118033988749894680 ) ) ;
#4781 = CARTESIAN_POINT ( 'NONE',  ( 2.624999999999996891, -28.29166666666666785, 4.546633369868304797 ) ) ;
#4782 = CARTESIAN_POINT ( 'NONE',  ( -3.492485675378535603, -6.549340926099361582, -1.467888652719048670 ) ) ;
#4783 = CARTESIAN_POINT ( 'NONE',  ( 0.000000000000000000, -53.00000000000000000, 0.000000000000000000 ) ) ;
#4784 = DIRECTION ( 'NONE',  ( 0.000000000000000000, 1.000000000000000000, 0.000000000000000000 ) ) ;
#4785 = PRODUCT_CONTEXT ( 'NONE', #5448, 'mechanical' ) ;
#4786 = CARTESIAN_POINT ( 'NONE',  ( -5.385316468750001029, -29.09895833299193058, -3.109213912904136734 ) ) ;
#4787 = CARTESIAN_POINT ( 'NONE',  ( -1.431606283892620235, -3.149340926099361671, -3.507514324621463953 ) ) ;
#4788 = DIRECTION ( 'NONE',  ( 0.000000000000000000, 1.000000000000000000, 0.000000000000000000 ) ) ;
#4789 = CARTESIAN_POINT ( 'NONE',  ( -2.692658234375000514, -27.15104166632526628, -4.663820869356205989 ) ) ;
#4790 = CARTESIAN_POINT ( 'NONE',  ( 3.992485675378568910, -5.450659073900638418, -1.674995433905514863 ) ) ;
#4791 = CARTESIAN_POINT ( 'NONE',  ( 2.033577675846918216E-14, -27.09375000068279604, 5.250000000000000888 ) ) ;
#4792 = CARTESIAN_POINT ( 'NONE',  ( 0.000000000000000000, 76.00000000000000000, 0.000000000000000000 ) ) ;
#4793 =( BOUNDED_SURFACE ( )  B_SPLINE_SURFACE ( 1, 2, ( 
 ( #3954, #5478, #1814, #8277, #4736, #8829, #8325, #2509, #7626, #555, #407, #1767, #3398, #4646, #7440, #1064, #3909, #6731, #6834, #1114, #3212, #6031, #8869, #2564, #5383, #8234, #459, #6133, #6970, #8505, #4226, #2749, #9103, #3484, #4912, #4952, #5658, #2086, #6227, #598, #6310, #1471, #4314, #1294, #6352, #9187, #725, #7057, #5570, #639, #4826, #7760, #2883, #32, #5701, #681, #3528, #3443, #7149, #4181, #6269, #773, #7808, #5612, #2000, #8545, #6397, #4266, #4135, #2129, #2838, #1425, #1382, #7013, #7715, #7101, #9146, #3572, #5529, #2701, #2792, #8374, #2172, #4993, #7850, #8460, #9058, #7671, #8415, #2041, #4865, #1341, #6631, #6442, #2313, #3805, #4501, #5745, #861, #5935, #1708, #6588, #2217, #3068, #8587, #1661, #7286, #7982, #3110, #5794, #168, #4448, #8081, #216, #7943, #8681, #7194, #4362, #4406, #3018, #959, #1517, #8635, #7378, #3710, #2265, #5043, #7236, #3618, #259, #121, #4546, #8775, #7898, #2405, #5235, #76, #2926, #5093, #8030, #6486, #5887, #8726, #1564, #819 ),
 ( #6535, #3661, #5843, #2970, #5139, #1609, #912, #3759, #2358, #5188, #7333, #7691, #436, #6162, #5549, #3461, #485, #3851, #2061, #576, #1275, #6205, #4028, #9126, #8939, #3421, #1231, #8259, #2722, #2590, #3330, #1891, #6250, #8351, #6862, #8988, #7607, #9036, #9082, #8395, #2678, #1004, #4716, #4071, #5591, #8435, #5410, #4113, #6947, #4846, #1976, #2636, #4763, #7557, #5508, #6993, #4158, #619, #4806, #7650, #1183, #4888, #8302, #5457, #6810, #2020, #534, #6112, #6290, #1316, #2771, #1935, #3283, #6909, #3374, #56, #8525, #12, #5721, #4973, #6463, #7038, #4202, #2153, #662, #4336, #5017, #1542, #749, #3640, #2243, #2947, #7827, #6329, #3593, #4383, #1363, #6418, #7918, #8610, #3506, #1445, #838, #5819, #1493, #9165, #7171, #2814, #5768, #2195, #2905, #7214, #701, #4290, #8566, #2997, #796, #2860, #7873, #96, #5064, #3684, #6510, #146, #8658, #5678, #2289, #7740, #5634, #8484, #2106, #4245, #7125, #4931, #7787, #1406, #7079, #3549, #6370, #8153, #283, #3785, #192, #5911, #4615 ) ),
 .UNSPECIFIED., .F., .F., .F. ) 
 B_SPLINE_SURFACE_WITH_KNOTS ( ( 2, 2 ),
 ( 3, 2, 2, 2, 2, 2, 2, 2, 2, 2, 2, 2, 2, 2, 2, 2, 2, 2, 2, 2, 2, 2, 2, 2, 2, 2, 2, 2, 2, 2, 2, 2, 2, 2, 2, 2, 2, 2, 2, 2, 2, 2, 2, 2, 2, 2, 2, 2, 2, 2, 2, 2, 2, 2, 2, 2, 2, 2, 2, 2, 2, 2, 2, 2, 2, 2, 2, 2, 2, 2, 2, 2, 3 ),
 ( 0.000000000000000000, 1.000000000000000000 ),
 ( 0.000000000000000000, 0.01388888888888888812, 0.02777777777777777624, 0.04166666666666666435, 0.05555555555555555247, 0.06944444444444444753, 0.08333333333333332871, 0.09722222222222222376, 0.1111111111111111049, 0.1250000000000000000, 0.1388888888888888951, 0.1527777777777777901, 0.1666666666666666574, 0.1805555555555555525, 0.1944444444444444475, 0.2083333333333333426, 0.2222222222222222099, 0.2361111111111111049, 0.2500000000000000000, 0.2638888888888888951, 0.2777777777777777901, 0.2916666666666666852, 0.3055555555555555802, 0.3194444444444444198, 0.3333333333333333148, 0.3472222222222222099, 0.3611111111111111049, 0.3750000000000000000, 0.3888888888888888951, 0.4027777777777777901, 0.4166666666666666852, 0.4305555555555555802, 0.4444444444444444198, 0.4583333333333333148, 0.4722222222222222099, 0.4861111111111111049, 0.5000000000000000000, 0.5138888888888888395, 0.5277777777777777901, 0.5416666666666666297, 0.5555555555555555802, 0.5694444444444444198, 0.5833333333333333703, 0.5972222222222222099, 0.6111111111111111605, 0.6250000000000000000, 0.6388888888888888395, 0.6527777777777777901, 0.6666666666666666297, 0.6805555555555555802, 0.6944444444444444198, 0.7083333333333333703, 0.7222222222222222099, 0.7361111111111111605, 0.7500000000000000000, 0.7638888888888888395, 0.7777777777777777901, 0.7916666666666666297, 0.8055555555555555802, 0.8194444444444444198, 0.8333333333333333703, 0.8472222222222222099, 0.8611111111111111605, 0.8750000000000000000, 0.8888888888888888395, 0.9027777777777777901, 0.9166666666666666297, 0.9305555555555555802, 0.9444444444444444198, 0.9583333333333333703, 0.9722222222222222099, 0.9861111111111111605, 1.000000000000000000 ),
 .UNSPECIFIED. ) 
 GEOMETRIC_REPRESENTATION_ITEM ( )  RATIONAL_B_SPLINE_SURFACE ( (
 ( 1.000000000000000000, 0.8660254037844387076, 1.000000000000000000, 0.8660254037844387076, 1.000000000000000000, 0.8660254037844387076, 1.000000000000000000, 0.8660254037844387076, 1.000000000000000000, 0.8660254037844387076, 1.000000000000000000, 0.8660254037844387076, 1.000000000000000000, 0.8660254037844387076, 1.000000000000000000, 0.8660254037844387076, 1.000000000000000000, 0.8660254037844387076, 1.000000000000000000, 0.8660254037844387076, 1.000000000000000000, 0.8660254037844387076, 1.000000000000000000, 0.8660254037844387076, 1.000000000000000000, 0.8660254037844387076, 1.000000000000000000, 0.8660254037844387076, 1.000000000000000000, 0.8660254037844387076, 1.000000000000000000, 0.8660254037844387076, 1.000000000000000000, 0.8660254037844387076, 1.000000000000000000, 0.8660254037844387076, 1.000000000000000000, 0.8660254037844387076, 1.000000000000000000, 0.8660254037844387076, 1.000000000000000000, 0.8660254037844387076, 1.000000000000000000, 0.8660254037844387076, 1.000000000000000000, 0.8660254037844387076, 1.000000000000000000, 0.8660254037844387076, 1.000000000000000000, 0.8660254037844387076, 1.000000000000000000, 0.8660254037844387076, 1.000000000000000000, 0.8660254037844387076, 1.000000000000000000, 0.8660254037844387076, 1.000000000000000000, 0.8660254037844387076, 1.000000000000000000, 0.8660254037844387076, 1.000000000000000000, 0.8660254037844387076, 1.000000000000000000, 0.8660254037844387076, 1.000000000000000000, 0.8660254037844387076, 1.000000000000000000, 0.8660254037844387076, 1.000000000000000000, 0.8660254037844387076, 1.000000000000000000, 0.8660254037844387076, 1.000000000000000000, 0.8660254037844387076, 1.000000000000000000, 0.8660254037844387076, 1.000000000000000000, 0.8660254037844387076, 1.000000000000000000, 0.8660254037844387076, 1.000000000000000000, 0.8660254037844387076, 1.000000000000000000, 0.8660254037844387076, 1.000000000000000000, 0.8660254037844387076, 1.000000000000000000, 0.8660254037844387076, 1.000000000000000000, 0.8660254037844387076, 1.000000000000000000, 0.8660254037844387076, 1.000000000000000000, 0.8660254037844387076, 1.000000000000000000, 0.8660254037844387076, 1.000000000000000000, 0.8660254037844387076, 1.000000000000000000, 0.8660254037844387076, 1.000000000000000000, 0.8660254037844387076, 1.000000000000000000, 0.8660254037844387076, 1.000000000000000000, 0.8660254037844387076, 1.000000000000000000, 0.8660254037844387076, 1.000000000000000000, 0.8660254037844387076, 1.000000000000000000, 0.8660254037844387076, 1.000000000000000000, 0.8660254037844387076, 1.000000000000000000, 0.8660254037844387076, 1.000000000000000000, 0.8660254037844387076, 1.000000000000000000, 0.8660254037844387076, 1.000000000000000000, 0.8660254037844387076, 1.000000000000000000, 0.8660254037844387076, 1.000000000000000000, 0.8660254037844387076, 1.000000000000000000, 0.8660254037844387076, 1.000000000000000000, 0.8660254037844387076, 1.000000000000000000, 0.8660254037844387076, 1.000000000000000000, 0.8660254037844387076, 1.000000000000000000, 0.8660254037844387076, 1.000000000000000000, 0.8660254037844387076, 1.000000000000000000, 0.8660254037844387076, 1.000000000000000000, 0.8660254037844387076, 1.000000000000000000, 0.8660254037844387076, 1.000000000000000000),
 ( 1.000000000000000000, 0.8660254037844387076, 1.000000000000000000, 0.8660254037844387076, 1.000000000000000000, 0.8660254037844387076, 1.000000000000000000, 0.8660254037844387076, 1.000000000000000000, 0.8660254037844387076, 1.000000000000000000, 0.8660254037844387076, 1.000000000000000000, 0.8660254037844387076, 1.000000000000000000, 0.8660254037844387076, 1.000000000000000000, 0.8660254037844387076, 1.000000000000000000, 0.8660254037844387076, 1.000000000000000000, 0.8660254037844387076, 1.000000000000000000, 0.8660254037844387076, 1.000000000000000000, 0.8660254037844387076, 1.000000000000000000, 0.8660254037844387076, 1.000000000000000000, 0.8660254037844387076, 1.000000000000000000, 0.8660254037844387076, 1.000000000000000000, 0.8660254037844387076, 1.000000000000000000, 0.8660254037844387076, 1.000000000000000000, 0.8660254037844387076, 1.000000000000000000, 0.8660254037844387076, 1.000000000000000000, 0.8660254037844387076, 1.000000000000000000, 0.8660254037844387076, 1.000000000000000000, 0.8660254037844387076, 1.000000000000000000, 0.8660254037844387076, 1.000000000000000000, 0.8660254037844387076, 1.000000000000000000, 0.8660254037844387076, 1.000000000000000000, 0.8660254037844387076, 1.000000000000000000, 0.8660254037844387076, 1.000000000000000000, 0.8660254037844387076, 1.000000000000000000, 0.8660254037844387076, 1.000000000000000000, 0.8660254037844387076, 1.000000000000000000, 0.8660254037844387076, 1.000000000000000000, 0.8660254037844387076, 1.000000000000000000, 0.8660254037844387076, 1.000000000000000000, 0.8660254037844387076, 1.000000000000000000, 0.8660254037844387076, 1.000000000000000000, 0.8660254037844387076, 1.000000000000000000, 0.8660254037844387076, 1.000000000000000000, 0.8660254037844387076, 1.000000000000000000, 0.8660254037844387076, 1.000000000000000000, 0.8660254037844387076, 1.000000000000000000, 0.8660254037844387076, 1.000000000000000000, 0.8660254037844387076, 1.000000000000000000, 0.8660254037844387076, 1.000000000000000000, 0.8660254037844387076, 1.000000000000000000, 0.8660254037844387076, 1.000000000000000000, 0.8660254037844387076, 1.000000000000000000, 0.8660254037844387076, 1.000000000000000000, 0.8660254037844387076, 1.000000000000000000, 0.8660254037844387076, 1.000000000000000000, 0.8660254037844387076, 1.000000000000000000, 0.8660254037844387076, 1.000000000000000000, 0.8660254037844387076, 1.000000000000000000, 0.8660254037844387076, 1.000000000000000000, 0.8660254037844387076, 1.000000000000000000, 0.8660254037844387076, 1.000000000000000000, 0.8660254037844387076, 1.000000000000000000, 0.8660254037844387076, 1.000000000000000000, 0.8660254037844387076, 1.000000000000000000, 0.8660254037844387076, 1.000000000000000000, 0.8660254037844387076, 1.000000000000000000, 0.8660254037844387076, 1.000000000000000000, 0.8660254037844387076, 1.000000000000000000, 0.8660254037844387076, 1.000000000000000000, 0.8660254037844387076, 1.000000000000000000, 0.8660254037844387076, 1.000000000000000000, 0.8660254037844387076, 1.000000000000000000, 0.8660254037844387076, 1.000000000000000000, 0.8660254037844387076, 1.000000000000000000, 0.8660254037844387076, 1.000000000000000000, 0.8660254037844387076, 1.000000000000000000, 0.8660254037844387076, 1.000000000000000000) ) ) 
 REPRESENTATION_ITEM ( '' )  SURFACE ( )  );
#4794 = EDGE_LOOP ( 'NONE', ( #2401, #4469, #291, #4328 ) ) ;
#4795 =( NAMED_UNIT ( * ) SI_UNIT ( $, .STERADIAN. ) SOLID_ANGLE_UNIT ( ) );
#4796 = CARTESIAN_POINT ( 'NONE',  ( 2.625000000000002220, -28.66666666666666785, 4.546633369868302132 ) ) ;
#4797 = VECTOR ( 'NONE', #1271, 1000.000000000000000 ) ;
#4798 = CARTESIAN_POINT ( 'NONE',  ( -2.557341765625002594, -27.69270833367473017, 4.429445870380399164 ) ) ;
#4799 = CARTESIAN_POINT ( 'NONE',  ( 3.000000000000000444, -2.649340926099361671, 0.01814118441320859698 ) ) ;
#4800 = CARTESIAN_POINT ( 'NONE',  ( 0.000000000000000000, 70.00000000000000000, -3.000000000000000444 ) ) ;
#4801 = CARTESIAN_POINT ( 'NONE',  ( 2.625000000000000444, -29.95833333333333215, -4.546633369868303021 ) ) ;
#4802 = CARTESIAN_POINT ( 'NONE',  ( 0.000000000000000000, 69.99999999999998579, 0.000000000000000000 ) ) ;
#4803 = EDGE_CURVE ( 'NONE', #4496, #4617, #7401, .T. ) ;
#4804 = CIRCLE ( 'NONE', #7632, 2.750000000000000000 ) ;
#4805 = CARTESIAN_POINT ( 'NONE',  ( 2.557341765624996821, -29.71354166700806232, 4.429445870380401828 ) ) ;
#4806 = CARTESIAN_POINT ( 'NONE',  ( 2.557341765624996821, -28.71354166700806587, 4.429445870380401828 ) ) ;
#4807 = CARTESIAN_POINT ( 'NONE',  ( -1.406733260263384411, -28.80133545031537068, -5.250000000000006217 ) ) ;
#4808 = CARTESIAN_POINT ( 'NONE',  ( -2.624999999999996891, -28.89583333265053611, 4.546633369868304797 ) ) ;
#4809 = CARTESIAN_POINT ( 'NONE',  ( 6.972266317189433020E-16, -28.68749999999999645, -5.250000000000000000 ) ) ;
#4810 = AXIS2_PLACEMENT_3D ( 'NONE', #308, #1006, #7238 ) ;
#4811 = DIRECTION ( 'NONE',  ( 0.000000000000000000, 1.000000000000000000, 0.000000000000000000 ) ) ;
#4812 = CARTESIAN_POINT ( 'NONE',  ( -2.692658234375000514, -29.90104166632526983, -4.663820869356205989 ) ) ;
#4813 = CARTESIAN_POINT ( 'NONE',  ( -3.507514324621464397, -0.3493409260993610710, 1.431606283892619347 ) ) ;
#4814 = CARTESIAN_POINT ( 'NONE',  ( 3.507514324621465285, -1.149340926099361226, -1.431606283892619125 ) ) ;
#4815 = EDGE_CURVE ( 'NONE', #7322, #5643, #3101, .T. ) ;
#4816 = ORIENTED_EDGE ( 'NONE', *, *, #5422, .F. ) ;
#4817 = CARTESIAN_POINT ( 'NONE',  ( 5.204748896376250699E-16, -30.00000000000000000, -4.250000000000000000 ) ) ;
#4818 = CARTESIAN_POINT ( 'NONE',  ( 2.557341765625000818, -29.81770833367473372, -4.429445870380400052 ) ) ;
#4819 = CARTESIAN_POINT ( 'NONE',  ( 1.142306659890740623E-15, -28.79687499965860198, 6.218427825808274356 ) ) ;
#4820 = VERTEX_POINT ( 'NONE', #5784 ) ;
#4821 = CARTESIAN_POINT ( 'NONE',  ( -3.807688866302469071E-16, -29.14062499965860553, -6.218427825808274356 ) ) ;
#4822 = CARTESIAN_POINT ( 'NONE',  ( 3.500000000000000000, -0.5506590739006389512, -0.01814118441313969030 ) ) ;
#4823 = CARTESIAN_POINT ( 'NONE',  ( 2.033577675846918216E-14, -27.31250000000000355, 5.250000000000000888 ) ) ;
#4824 = CARTESIAN_POINT ( 'NONE',  ( 0.000000000000000000, -9.999999999999998224, 2.750000000000000000 ) ) ;
#4825 = DIRECTION ( 'NONE',  ( 1.000000000000000000, 0.000000000000000000, 0.000000000000000000 ) ) ;
#4826 = CARTESIAN_POINT ( 'NONE',  ( 2.557341765625000818, -28.81770833367473017, -4.429445870380400052 ) ) ;
#4827 = CARTESIAN_POINT ( 'NONE',  ( 5.250000000000000000, -28.31249999931720396, -6.429395695523604153E-16 ) ) ;
#4828 = CONTEXT_DEPENDENT_SHAPE_REPRESENTATION ( #2613, #5922 ) ;
#4829 = CARTESIAN_POINT ( 'NONE',  ( -5.385316468750000141, -29.57812499965859843, 0.000000000000000000 ) ) ;
#4830 = CARTESIAN_POINT ( 'NONE',  ( -3.000000000000000444, -0.2493409260993614540, -0.01814118441320822922 ) ) ;
#4831 = CARTESIAN_POINT ( 'NONE',  ( -2.624999999999996891, -27.95833333333333215, 4.546633369868304797 ) ) ;
#4832 = CARTESIAN_POINT ( 'NONE',  ( 5.385316468749999252, -29.18229166632526983, -3.109213912904139399 ) ) ;
#4833 = CARTESIAN_POINT ( 'NONE',  ( -2.841254879263473310, -5.950659073900640195, -2.815599370228907716 ) ) ;
#4834 = CARTESIAN_POINT ( 'NONE',  ( -5.250000000000000000, -27.15625000068279604, -6.429395695523604153E-16 ) ) ;
#4835 = LINE ( 'NONE', #8244, #7738 ) ;
#4836 = EDGE_CURVE ( 'NONE', #1200, #4378, #810, .T. ) ;
#4837 = ORIENTED_EDGE ( 'NONE', *, *, #1228, .F. ) ;
#4838 = CARTESIAN_POINT ( 'NONE',  ( -2.625000000000000444, -28.29166666666666785, -4.546633369868303021 ) ) ;
#4839 = CARTESIAN_POINT ( 'NONE',  ( 2.557341765625000818, -27.31770833367473017, -4.429445870380400052 ) ) ;
#4840 = CARTESIAN_POINT ( 'NONE',  ( 3.000000000000000444, -5.849340926099360516, 0.01814118441320859698 ) ) ;
#4841 = CARTESIAN_POINT ( 'NONE',  ( -5.114683531249999859, -27.31770833367473017, -2.952963913586935440 ) ) ;
#4842 = CYLINDRICAL_SURFACE ( 'NONE', #190, 5.250000000000000000 ) ;
#4843 =( BOUNDED_CURVE ( )  B_SPLINE_CURVE ( 2, ( #4809, #5461, #6814, #7561, #2543, #6764, #4676, #1142, #440 ),
 .UNSPECIFIED., .F., .T. ) 
 B_SPLINE_CURVE_WITH_KNOTS ( ( 3, 2, 2, 2, 3 ),
 ( 0.4375000000000000000, 0.4444444444444444198, 0.4583333333333333148, 0.4722222222222222099, 0.4791666666666666852 ),
 .UNSPECIFIED. ) 
 CURVE ( )  GEOMETRIC_REPRESENTATION_ITEM ( )  RATIONAL_B_SPLINE_CURVE ( ( 0.9330127018922194093, 0.9330127018922194093, 1.000000000000000000, 0.8660254037844387076, 1.000000000000000000, 0.8660254037844387076, 1.000000000000000000, 0.9330127018922190762, 0.9330127018922194093 ) ) 
 REPRESENTATION_ITEM ( '' )  );
#4844 = CARTESIAN_POINT ( 'NONE',  ( -5.114683531250000748, -29.31770833367473017, -2.952963913586935440 ) ) ;
#4845 = DIRECTION ( 'NONE',  ( 0.000000000000000000, -0.000000000000000000, 1.000000000000000000 ) ) ;
#4846 = CARTESIAN_POINT ( 'NONE',  ( 5.114683531249999859, -28.90104166700806942, -2.952963913586932776 ) ) ;
#4847 = LINE ( 'NONE', #7955, #279 ) ;
#4848 = CARTESIAN_POINT ( 'NONE',  ( 2.624999999999998668, -29.02083333265053611, -4.546633369868303021 ) ) ;
#4849 = FACE_OUTER_BOUND ( 'NONE', #329, .T. ) ;
#4850 = CARTESIAN_POINT ( 'NONE',  ( -5.250000000000000000, -27.18749999931720396, 0.000000000000000000 ) ) ;
#4851 = CARTESIAN_POINT ( 'NONE',  ( 0.01814118441321408565, -4.649340926099361226, -3.500000000000000000 ) ) ;
#4852 = CARTESIAN_POINT ( 'NONE',  ( -3.500000000000000000, -0.2493409260993610654, -0.01814118441321344033 ) ) ;
#4853 = ORIENTED_EDGE ( 'NONE', *, *, #3049, .F. ) ;
#4854 = LINE ( 'NONE', #7700, #4459 ) ;
#4855 = CARTESIAN_POINT ( 'NONE',  ( 5.114683531249999859, -29.58854166700806232, -2.952963913586932776 ) ) ;
#4856 = CARTESIAN_POINT ( 'NONE',  ( 5.385316468750001029, -30.00520833299193768, 3.109213912904135846 ) ) ;
#4857 = VERTEX_POINT ( 'NONE', #160 ) ;
#4858 = CARTESIAN_POINT ( 'NONE',  ( 2.692658234374998738, -29.91145833299193413, -4.663820869356206877 ) ) ;
#4859 = CARTESIAN_POINT ( 'NONE',  ( 1.674995433905515085, -0.2506590739006385182, 3.992485675378568022 ) ) ;
#4860 = LINE ( 'NONE', #4220, #5488 ) ;
#4861 = EDGE_CURVE ( 'NONE', #6553, #6037, #6437, .T. ) ;
#4862 = DIRECTION ( 'NONE',  ( 0.000000000000000000, 0.000000000000000000, -1.000000000000000000 ) ) ;
#4863 = DIRECTION ( 'NONE',  ( 0.000000000000000000, 0.000000000000000000, -1.000000000000000000 ) ) ;
#4864 = CARTESIAN_POINT ( 'NONE',  ( 2.625000000000000444, -27.73958333401612819, -4.546633369868303021 ) ) ;
#4865 = CARTESIAN_POINT ( 'NONE',  ( -5.114683531250000748, -27.98437500034139802, -6.263680815196995234E-16 ) ) ;
#4866 = CARTESIAN_POINT ( 'NONE',  ( 0.000000000000000000, -20.00000000000000000, 2.500000000000000444 ) ) ;
#4867 = CONTEXT_DEPENDENT_SHAPE_REPRESENTATION ( #991, #8748 ) ;
#4868 = CARTESIAN_POINT ( 'NONE',  ( 2.692658234374998738, -28.44270833299193413, -4.663820869356206877 ) ) ;
#4869 = CARTESIAN_POINT ( 'NONE',  ( -1.975475456537005874E-15, -29.09375000068278894, 5.250000000000000000 ) ) ;
#4870 = CARTESIAN_POINT ( 'NONE',  ( -2.134148098076978251, -6.849340926099361404, 2.108492589042307408 ) ) ;
#4871 = EDGE_CURVE ( 'NONE', #3470, #3226, #1979, .T. ) ;
#4872 = CARTESIAN_POINT ( 'NONE',  ( 2.300847884672513123E-14, -28.21875000068279604, -5.250000000000000000 ) ) ;
#4873 = CARTESIAN_POINT ( 'NONE',  ( -5.385316468750001029, -29.84895833299193413, -3.109213912904136734 ) ) ;
#4874 = CARTESIAN_POINT ( 'NONE',  ( -4.007514324621431534, -4.450659073900638418, -1.638713065079248521 ) ) ;
#4875 = CARTESIAN_POINT ( 'NONE',  ( 1.185285273922203525E-14, -29.18749999999999645, -5.249999999999999112 ) ) ;
#4876 = CARTESIAN_POINT ( 'NONE',  ( 1.406733260263402174, -27.30133545031537068, 5.249999999999995559 ) ) ;
#4877 = AXIS2_PLACEMENT_3D ( 'NONE', #7765, #3577, #1387 ) ;
#4878 = CARTESIAN_POINT ( 'NONE',  ( 0.000000000000000000, -20.00000000000000000, 0.000000000000000000 ) ) ;
#4879 = ORIENTED_EDGE ( 'NONE', *, *, #1398, .T. ) ;
#4880 = CARTESIAN_POINT ( 'NONE',  ( 5.385316468750000141, -27.20312499965860198, -6.595110575850215044E-16 ) ) ;
#4881 = CARTESIAN_POINT ( 'NONE',  ( 5.114683531250000748, -27.10937500034139802, 0.000000000000000000 ) ) ;
#4882 = CARTESIAN_POINT ( 'NONE',  ( 1.260781871532495657, -7.749340926099362648, -2.992485675378538268 ) ) ;
#4883 = CARTESIAN_POINT ( 'NONE',  ( -2.557341765625002594, -27.50520833367473017, 4.429445870380399164 ) ) ;
#4884 = DIRECTION ( 'NONE',  ( 0.000000000000000000, -1.000000000000000000, 0.000000000000000000 ) ) ;
#4885 = CARTESIAN_POINT ( 'NONE',  ( -5.114683531250000748, -29.81770833367473372, -2.952963913586935440 ) ) ;
#4886 = MECHANICAL_DESIGN_GEOMETRIC_PRESENTATION_REPRESENTATION (  '', ( #2525 ), #880 ) ;
#4887 = CARTESIAN_POINT ( 'NONE',  ( 0.000000000000000000, 70.00000000000000000, 0.000000000000000000 ) ) ;
#4888 = CARTESIAN_POINT ( 'NONE',  ( 5.114683531249999859, -28.65104166700806587, -2.952963913586932776 ) ) ;
#4889 = VECTOR ( 'NONE', #5790, 1000.000000000000000 ) ;
#4890 = CARTESIAN_POINT ( 'NONE',  ( 3.367778697655221012E-16, -9.000000000000000000, -2.750000000000000000 ) ) ;
#4891 = CARTESIAN_POINT ( 'NONE',  ( 2.624999999999998668, -29.52083333265053611, -4.546633369868303021 ) ) ;
#4892 = DIRECTION ( 'NONE',  ( -0.000000000000000000, 1.000000000000000000, -0.000000000000000000 ) ) ;
#4893 = CARTESIAN_POINT ( 'NONE',  ( 5.249999999999997335, -28.52083333333333215, 3.031088913245538308 ) ) ;
#4894 = CARTESIAN_POINT ( 'NONE',  ( -3.500000000000000000, -5.049340926099361582, -0.01814118441321344033 ) ) ;
#4895 = CARTESIAN_POINT ( 'NONE',  ( 1.431606283892619125, -3.949340926099361049, 3.507514324621464397 ) ) ;
#4896 = ORIENTED_EDGE ( 'NONE', *, *, #7076, .F. ) ;
#4897 = CARTESIAN_POINT ( 'NONE',  ( 0.000000000000000000, 0.000000000000000000, 2.500000000000000444 ) ) ;
#4898 = AXIS2_PLACEMENT_3D ( 'NONE', #84, #6495, #8642 ) ;
#4899 = CARTESIAN_POINT ( 'NONE',  ( -2.625000000000002220, -26.86458333401613174, 4.546633369868302132 ) ) ;
#4900 = ADVANCED_FACE ( 'NONE', ( #2681 ), #2579, .T. ) ;
#4901 = ORIENTED_EDGE ( 'NONE', *, *, #8274, .F. ) ;
#4902 = CARTESIAN_POINT ( 'NONE',  ( 5.385316468750000141, -29.45312499965859843, -6.595110575850215044E-16 ) ) ;
#4903 = CARTESIAN_POINT ( 'NONE',  ( 3.992485675378568910, -0.6506590739006385959, -1.674995433905514863 ) ) ;
#4904 = DIRECTION ( 'NONE',  ( 0.000000000000000000, 1.000000000000000000, 0.000000000000000000 ) ) ;
#4905 = AXIS2_PLACEMENT_3D ( 'NONE', #3315, #6000, #7353 ) ;
#4906 = EDGE_LOOP ( 'NONE', ( #468, #968, #8047, #3183 ) ) ;
#4907 = EDGE_CURVE ( 'NONE', #8178, #5951, #8363, .T. ) ;
#4908 = CARTESIAN_POINT ( 'NONE',  ( -5.250000000000000000, -27.09374999965859843, 0.000000000000000000 ) ) ;
#4909 = DIRECTION ( 'NONE',  ( 0.000000000000000000, -1.000000000000000000, 0.000000000000000000 ) ) ;
#4910 = CARTESIAN_POINT ( 'NONE',  ( 5.250000000000000000, -27.78125000068279604, 0.000000000000000000 ) ) ;
#4911 = VECTOR ( 'NONE', #7010, 1000.000000000000000 ) ;
#4912 = CARTESIAN_POINT ( 'NONE',  ( 2.557341765624996821, -29.15104166700806587, 4.429445870380401828 ) ) ;
#4913 = CARTESIAN_POINT ( 'NONE',  ( 1.045839947578414884E-14, -28.24999999931720041, -5.250000000000000000 ) ) ;
#4914 = CARTESIAN_POINT ( 'NONE',  ( 2.161402558328724325E-14, -28.74999999931720751, -5.250000000000000000 ) ) ;
#4915 = CARTESIAN_POINT ( 'NONE',  ( 2.992485675378538712, -7.349340926099363180, 1.260781871532494103 ) ) ;
#4916 = CARTESIAN_POINT ( 'NONE',  ( 2.624999999999998668, -28.58333333333333215, -4.546633369868303021 ) ) ;
#4917 =( BOUNDED_CURVE ( )  B_SPLINE_CURVE ( 2, ( #7162, #7864, #928, #3082, #5157, #1533, #2282, #739, #1485 ),
 .UNSPECIFIED., .F., .F. ) 
 B_SPLINE_CURVE_WITH_KNOTS ( ( 3, 2, 2, 2, 3 ),
 ( 0.06250000000000000000, 0.06944444444444444753, 0.08333333333333332871, 0.09722222222222222376, 0.1041666666666666713 ),
 .UNSPECIFIED. ) 
 CURVE ( )  GEOMETRIC_REPRESENTATION_ITEM ( )  RATIONAL_B_SPLINE_CURVE ( ( 0.9330127018922194093, 0.9330127018922194093, 1.000000000000000000, 0.8660254037844387076, 1.000000000000000000, 0.8660254037844387076, 1.000000000000000000, 0.9330127018922192983, 0.9330127018922194093 ) ) 
 REPRESENTATION_ITEM ( '' )  );
#4918 = CARTESIAN_POINT ( 'NONE',  ( 1.142306659890740623E-15, -29.51562499965859487, 6.218427825808274356 ) ) ;
#4919 = CARTESIAN_POINT ( 'NONE',  ( 2.841254879263473310, -0.3506590739006385515, 2.815599370228907272 ) ) ;
#4920 = CARTESIAN_POINT ( 'NONE',  ( 0.000000000000000000, -9.999999999999998224, 0.000000000000000000 ) ) ;
#4921 = PRODUCT ( 'lead sleeve', 'lead sleeve', '', ( #7531 ) ) ;
#4922 = EDGE_LOOP ( 'NONE', ( #9094, #1092 ) ) ;
#4923 = CARTESIAN_POINT ( 'NONE',  ( -5.249999999999999112, -29.47916666666666785, 3.031088913245538308 ) ) ;
#4924 = CARTESIAN_POINT ( 'NONE',  ( -2.557341765624999042, -27.27604166700806587, -4.429445870380400052 ) ) ;
#4925 = CARTESIAN_POINT ( 'NONE',  ( 3.007514324621463508, -7.549340926099361582, -1.224499502706076770 ) ) ;
#4926 = CARTESIAN_POINT ( 'NONE',  ( 2.625000000000000444, -28.70833333333333215, -4.546633369868303021 ) ) ;
#4927 = CARTESIAN_POINT ( 'NONE',  ( 0.000000000000000000, -30.00000000000000000, 0.000000000000000000 ) ) ;
#4928 = EDGE_CURVE ( 'NONE', #6454, #8645, #4843, .T. ) ;
#4929 = CARTESIAN_POINT ( 'NONE',  ( 5.114683531249998971, -29.19270833367473017, 2.952963913586936329 ) ) ;
#4930 = CIRCLE ( 'NONE', #2271, 3.794308781941904574 ) ;
#4931 = CARTESIAN_POINT ( 'NONE',  ( 5.114683531249999859, -27.15104166700806232, -2.952963913586932776 ) ) ;
#4932 = CARTESIAN_POINT ( 'NONE',  ( -5.250000000000000888, -28.38541666734946389, 3.031088913245533423 ) ) ;
#4933 = CARTESIAN_POINT ( 'NONE',  ( -5.249999999999999112, -28.91666666598386826, 3.031088913245538308 ) ) ;
#4934 = DIRECTION ( 'NONE',  ( -0.000000000000000000, -1.000000000000000000, -0.000000000000000000 ) ) ;
#4935 = AXIS2_PLACEMENT_3D ( 'NONE', #4132, #2506, #405 ) ;
#4936 = DIRECTION ( 'NONE',  ( 0.000000000000000000, -1.000000000000000000, 0.000000000000000000 ) ) ;
#4937 = CARTESIAN_POINT ( 'NONE',  ( 1.431606283892619125, -0.7493409260993610932, 3.507514324621464397 ) ) ;
#4938 =( LENGTH_UNIT ( ) NAMED_UNIT ( * ) SI_UNIT ( .MILLI., .METRE. ) );
#4939 = ORIENTED_EDGE ( 'NONE', *, *, #1307, .F. ) ;
#4940 = CARTESIAN_POINT ( 'NONE',  ( -2.625000000000000444, -28.97916666598386826, -4.546633369868303021 ) ) ;
#4941 = CARTESIAN_POINT ( 'NONE',  ( -1.084901341431563923E-15, -29.17187500034139802, 5.905927827173866440 ) ) ;
#4942 = ADVANCED_FACE ( 'NONE', ( #1187, #4031 ), #6165, .F. ) ;
#4943 = AXIS2_PLACEMENT_3D ( 'NONE', #7323, #950, #7935 ) ;
#4944 = ORIENTED_EDGE ( 'NONE', *, *, #2626, .T. ) ;
#4945 = CARTESIAN_POINT ( 'NONE',  ( -5.385316468749998364, -30.05729166632526628, 3.109213912904140287 ) ) ;
#4946 = CARTESIAN_POINT ( 'NONE',  ( 0.01814118441313467001, -1.750659073900638685, 4.000000000000000000 ) ) ;
#4947 = DIRECTION ( 'NONE',  ( 0.000000000000000000, 1.000000000000000000, 0.000000000000000000 ) ) ;
#4948 = ORIENTED_EDGE ( 'NONE', *, *, #957, .F. ) ;
#4949 = CARTESIAN_POINT ( 'NONE',  ( -2.625000000000002220, -27.58333333333333215, 4.546633369868302132 ) ) ;
#4950 = DIRECTION ( 'NONE',  ( 0.000000000000000000, 0.000000000000000000, -1.000000000000000000 ) ) ;
#4951 = CARTESIAN_POINT ( 'NONE',  ( 5.385316468750000141, -27.23437499965860198, -6.595110575850215044E-16 ) ) ;
#4952 = CARTESIAN_POINT ( 'NONE',  ( 5.114683531249998971, -29.13020833367473372, 2.952963913586936329 ) ) ;
#4953 = DIRECTION ( 'NONE',  ( 0.000000000000000000, 0.000000000000000000, -1.000000000000000000 ) ) ;
#4954 = ADVANCED_BREP_SHAPE_REPRESENTATION ( '', ( #8209, #888 ), #1745 ) ;
#4955 = CARTESIAN_POINT ( 'NONE',  ( -1.975475456537005874E-15, -28.84375000068279959, 5.250000000000000000 ) ) ;
#4956 = CARTESIAN_POINT ( 'NONE',  ( 2.108492589042307408, -5.649340926099361226, 2.134148098076978251 ) ) ;
#4957 = ADVANCED_FACE ( 'NONE', ( #4766 ), #3509, .F. ) ;
#4958 = CARTESIAN_POINT ( 'NONE',  ( 1.142306659890740623E-15, -28.54687499965860198, 6.218427825808274356 ) ) ;
#4959 = CARTESIAN_POINT ( 'NONE',  ( 4.007514324621432422, -5.250659073900638241, 1.638713065079246078 ) ) ;
#4960 = DIRECTION ( 'NONE',  ( 0.000000000000000000, -1.000000000000000000, 0.000000000000000000 ) ) ;
#4961 = APPLICATION_CONTEXT ( 'automotive_design' ) ;
#4962 = CARTESIAN_POINT ( 'NONE',  ( 0.000000000000000000, 74.00000000000001421, 0.000000000000000000 ) ) ;
#4963 = VERTEX_POINT ( 'NONE', #2774 ) ;
#4964 = PRESENTATION_STYLE_ASSIGNMENT (( #2143 ) ) ;
#4965 = CARTESIAN_POINT ( 'NONE',  ( 2.624999999999998668, -29.33333333333333215, -4.546633369868303021 ) ) ;
#4966 = EDGE_CURVE ( 'NONE', #8840, #2779, #6332, .T. ) ;
#4967 = DIRECTION ( 'NONE',  ( 0.000000000000000000, 1.000000000000000000, 0.000000000000000000 ) ) ;
#4968 = CARTESIAN_POINT ( 'NONE',  ( -0.01814118441320841310, -7.049340926099361582, 3.000000000000000444 ) ) ;
#4969 = ORIENTED_EDGE ( 'NONE', *, *, #4803, .F. ) ;
#4970 = CARTESIAN_POINT ( 'NONE',  ( 2.625000000000000444, -29.45833333333333215, -4.546633369868303021 ) ) ;
#4971 = EDGE_CURVE ( 'NONE', #874, #8929, #4163, .T. ) ;
#4972 = CARTESIAN_POINT ( 'NONE',  ( -5.114683531250001636, -29.77604166700806232, 2.952963913586931444 ) ) ;
#4973 = CARTESIAN_POINT ( 'NONE',  ( -5.114683531250000748, -28.27604166700806232, 2.952963913586931888 ) ) ;
#4974 = CARTESIAN_POINT ( 'NONE',  ( 1.113604000661152470E-15, -29.87499999931720396, 6.062177826491070398 ) ) ;
#4975 = CYLINDRICAL_SURFACE ( 'NONE', #7776, 5.250000000000000000 ) ;
#4976 = CARTESIAN_POINT ( 'NONE',  ( -3.121191317301271084, -3.932028342773297922E-17, 2.017464392153318187 ) ) ;
#4977 = CARTESIAN_POINT ( 'NONE',  ( 5.182341765625000818, -29.96093750017069723, 0.000000000000000000 ) ) ;
#4978 = CARTESIAN_POINT ( 'NONE',  ( -3.500000000000000000, -6.649340926099361226, -0.01814118441321344033 ) ) ;
#4979 = CARTESIAN_POINT ( 'NONE',  ( -2.462045979635576920, -8.049340926099361582, -2.487701488670255756 ) ) ;
#4980 = ORIENTED_EDGE ( 'NONE', *, *, #4815, .F. ) ;
#4981 = DIRECTION ( 'NONE',  ( 0.000000000000000000, 1.000000000000000000, 0.000000000000000000 ) ) ;
#4982 = CARTESIAN_POINT ( 'NONE',  ( 5.114683531249998971, -29.63020833367473017, 2.952963913586936329 ) ) ;
#4983 = ORIENTED_EDGE ( 'NONE', *, *, #3446, .F. ) ;
#4984 = ORIENTED_EDGE ( 'NONE', *, *, #7742, .T. ) ;
#4985 = CARTESIAN_POINT ( 'NONE',  ( -5.385316468749998364, -29.30729166632526983, 3.109213912904140287 ) ) ;
#4986 = CARTESIAN_POINT ( 'NONE',  ( -3.507514324621434199, -6.050659073900638951, -1.431606283892695064 ) ) ;
#4987 = CARTESIAN_POINT ( 'NONE',  ( 0.000000000000000000, -30.00000000000000000, 5.250000000000000000 ) ) ;
#4988 = EDGE_LOOP ( 'NONE', ( #111, #8103, #4536, #6582 ) ) ;
#4989 = PRODUCT_DEFINITION_SHAPE ( 'NONE', 'NONE',  #3942 ) ;
#4990 = CARTESIAN_POINT ( 'NONE',  ( -1.406733260263402174, -28.94866454968462577, 5.249999999999995559 ) ) ;
#4991 = DIRECTION ( 'NONE',  ( 0.000000000000000000, 0.000000000000000000, 1.000000000000000000 ) ) ;
#4992 = CYLINDRICAL_SURFACE ( 'NONE', #3139, 2.549999999999999822 ) ;
#4993 = CARTESIAN_POINT ( 'NONE',  ( 5.114683531249998971, -28.13020833367473017, 2.952963913586936329 ) ) ;
#4994 = CARTESIAN_POINT ( 'NONE',  ( -3.492485675378536047, -1.749340926099361093, -1.467888652719048670 ) ) ;
#4995 = FACE_OUTER_BOUND ( 'NONE', #974, .T. ) ;
#4996 = CARTESIAN_POINT ( 'NONE',  ( -2.108492589042306964, -4.849340926099359628, -2.134148098076978251 ) ) ;
#4997 = CARTESIAN_POINT ( 'NONE',  ( 2.161402558328724325E-14, -29.74999999931720396, -5.250000000000000000 ) ) ;
#4998 = PRODUCT_DEFINITION_FORMATION_WITH_SPECIFIED_SOURCE ( 'ANY', '', #4921, .NOT_KNOWN. ) ;
#4999 = CARTESIAN_POINT ( 'NONE',  ( -5.385316468750000141, -27.60937499965860198, 0.000000000000000000 ) ) ;
#5000 = CARTESIAN_POINT ( 'NONE',  ( 1.638713065079161924, -3.949340926099361493, 4.007514324621467949 ) ) ;
#5001 = DIRECTION ( 'NONE',  ( 0.000000000000000000, 0.000000000000000000, -1.000000000000000000 ) ) ;
#5002 = CARTESIAN_POINT ( 'NONE',  ( -5.250000000000000888, -27.63541666734946389, 3.031088913245533423 ) ) ;
#5003 = ORIENTED_EDGE ( 'NONE', *, *, #7886, .T. ) ;
#5004 = FILL_AREA_STYLE_COLOUR ( '', #7846 ) ;
#5005 = CARTESIAN_POINT ( 'NONE',  ( -3.712013335537174572E-16, -29.81250000000000000, -6.062177826491070398 ) ) ;
#5006 = EDGE_CURVE ( 'NONE', #8385, #8014, #3595, .T. ) ;
#5007 = VERTEX_POINT ( 'NONE', #704 ) ;
#5008 = CARTESIAN_POINT ( 'NONE',  ( -5.385316468750001029, -27.59895833299193413, -3.109213912904136734 ) ) ;
#5009 = CARTESIAN_POINT ( 'NONE',  ( 3.000000000000000444, -2.150659073900639484, -0.01814118441314496039 ) ) ;
#5010 = EDGE_LOOP ( 'NONE', ( #4592, #8857, #9090, #3655 ) ) ;
#5011 = CARTESIAN_POINT ( 'NONE',  ( 2.624999999999996891, -28.79166666666666785, 4.546633369868304797 ) ) ;
#5012 = FACE_OUTER_BOUND ( 'NONE', #7500, .T. ) ;
#5013 = EDGE_CURVE ( 'NONE', #6715, #4663, #8093, .T. ) ;
#5014 = CARTESIAN_POINT ( 'NONE',  ( 5.114683531249998971, -27.44270833367472662, 2.952963913586936329 ) ) ;
#5015 = CIRCLE ( 'NONE', #1024, 5.250000000000000000 ) ;
#5016 = ADVANCED_FACE ( 'NONE', ( #5638 ), #2907, .T. ) ;
#5017 = CARTESIAN_POINT ( 'NONE',  ( 2.557341765625000818, -28.13020833367473017, -4.429445870380400052 ) ) ;
#5018 = FACE_OUTER_BOUND ( 'NONE', #8154, .T. ) ;
#5019 = CARTESIAN_POINT ( 'NONE',  ( 0.000000000000000000, -28.00000000000000000, -4.199909308207393721 ) ) ;
#5020 = DIRECTION ( 'NONE',  ( -0.000000000000000000, 1.000000000000000000, -0.000000000000000000 ) ) ;
#5021 = DIRECTION ( 'NONE',  ( 0.000000000000000000, -0.000000000000000000, 1.000000000000000000 ) ) ;
#5022 = CARTESIAN_POINT ( 'NONE',  ( -2.462045979635576920, -8.049340926099361582, -2.487701488670255756 ) ) ;
#5023 = CARTESIAN_POINT ( 'NONE',  ( -3.507514324621464397, -5.149340926099360338, 1.431606283892619347 ) ) ;
#5024 = VERTEX_POINT ( 'NONE', #5019 ) ;
#5025 = VECTOR ( 'NONE', #7755, 1000.000000000000000 ) ;
#5026 = CARTESIAN_POINT ( 'NONE',  ( 1.431606283892694620, -7.250659073900639129, -3.507514324621433754 ) ) ;
#5027 = LINE ( 'NONE', #3794, #455 ) ;
#5028 = CARTESIAN_POINT ( 'NONE',  ( -5.114683531249999859, -28.75520833367473017, -2.952963913586935440 ) ) ;
#5029 = VERTEX_POINT ( 'NONE', #4205 ) ;
#5030 = ORIENTED_EDGE ( 'NONE', *, *, #6824, .T. ) ;
#5031 = CIRCLE ( 'NONE', #3269, 2.750000000000000000 ) ;
#5032 = CARTESIAN_POINT ( 'NONE',  ( 0.000000000000000000, -20.00000000000000000, 0.000000000000000000 ) ) ;
#5033 = CARTESIAN_POINT ( 'NONE',  ( 5.385316468750001029, -27.50520833299193413, 3.109213912904134958 ) ) ;
#5034 = CARTESIAN_POINT ( 'NONE',  ( -2.462045979635629323, -4.750659073900639129, 2.487701488670203798 ) ) ;
#5035 = DIRECTION ( 'NONE',  ( 0.000000000000000000, 0.000000000000000000, -1.000000000000000000 ) ) ;
#5036 = ORIENTED_EDGE ( 'NONE', *, *, #2605, .F. ) ;
#5037 = AXIS2_PLACEMENT_3D ( 'NONE', #8514, #7950, #2893 ) ;
#5038 = ADVANCED_FACE ( 'NONE', ( #7040 ), #2156, .F. ) ;
#5039 = CARTESIAN_POINT ( 'NONE',  ( -5.249999999999999112, -27.64583333333333215, -3.031088913245536975 ) ) ;
#5040 = CARTESIAN_POINT ( 'NONE',  ( 0.000000000000000000, -30.00000000000000000, -6.250000000000002665 ) ) ;
#5041 = EDGE_CURVE ( 'NONE', #2851, #4496, #5724, .T. ) ;
#5042 = CARTESIAN_POINT ( 'NONE',  ( 1.406733260263402174, -27.83258545099816672, 5.249999999999995559 ) ) ;
#5043 = CARTESIAN_POINT ( 'NONE',  ( -5.114683531250000748, -27.23437500034139802, -6.263680815196995234E-16 ) ) ;
#5044 = CIRCLE ( 'NONE', #8916, 2.500000000000000444 ) ;
#5045 = CARTESIAN_POINT ( 'NONE',  ( 1.406733260263393293, -27.76116454900182973, -5.250000000000000000 ) ) ;
#5046 = CARTESIAN_POINT ( 'NONE',  ( -3.000000000000000444, -1.849340926099361404, -0.01814118441320822922 ) ) ;
#5047 = DIRECTION ( 'NONE',  ( 0.000000000000000000, -1.000000000000000000, 0.000000000000000000 ) ) ;
#5048 = CARTESIAN_POINT ( 'NONE',  ( -3.807688866302469071E-16, -28.67187499965860198, -6.218427825808274356 ) ) ;
#5049 = CARTESIAN_POINT ( 'NONE',  ( -0.01814118441321889430, -0.6493409260993606713, 4.000000000000000000 ) ) ;
#5050 = ADVANCED_FACE ( 'NONE', ( #2024 ), #1409, .T. ) ;
#5051 = VECTOR ( 'NONE', #2878, 1000.000000000000000 ) ;
#5052 = CARTESIAN_POINT ( 'NONE',  ( 0.000000000000000000, 1.000000000000000888, 0.000000000000000000 ) ) ;
#5053 = DIRECTION ( 'NONE',  ( 0.000000000000000000, 1.000000000000000000, 0.000000000000000000 ) ) ;
#5054 = CARTESIAN_POINT ( 'NONE',  ( 0.000000000000000000, -9.000000000000000000, 0.000000000000000000 ) ) ;
#5055 = ORIENTED_EDGE ( 'NONE', *, *, #8607, .T. ) ;
#5056 = CARTESIAN_POINT ( 'NONE',  ( 5.385316468749999252, -27.18229166632526628, -3.109213912904139399 ) ) ;
#5057 = ORIENTED_EDGE ( 'NONE', *, *, #6326, .T. ) ;
#5058 = CARTESIAN_POINT ( 'NONE',  ( -5.385316468749998364, -27.30729166632526983, 3.109213912904140287 ) ) ;
#5059 = CARTESIAN_POINT ( 'NONE',  ( -2.462045979635629323, 0.04934092609936105434, 2.487701488670203798 ) ) ;
#5060 = ORIENTED_EDGE ( 'NONE', *, *, #6279, .F. ) ;
#5061 = CARTESIAN_POINT ( 'NONE',  ( -5.250000000000000888, -29.60416666666666430, 3.031088913245532979 ) ) ;
#5062 = CARTESIAN_POINT ( 'NONE',  ( 5.204748896376250699E-16, 75.00000000000000000, -4.250000000000000000 ) ) ;
#5063 = CARTESIAN_POINT ( 'NONE',  ( 5.114683531250000748, -27.90104166700806587, -2.952963913586932776 ) ) ;
#5064 = CARTESIAN_POINT ( 'NONE',  ( 5.114683531250000748, -27.42187500034139802, 0.000000000000000000 ) ) ;
#5065 = CARTESIAN_POINT ( 'NONE',  ( 3.616337804771879580E-16, -29.79687500034139447, -5.905927827173866440 ) ) ;
#5066 = PRODUCT ( 'cone', 'cone', '', ( #4648 ) ) ;
#5067 = CARTESIAN_POINT ( 'NONE',  ( 3.492485675378536047, -4.149340926099361226, 1.467888652719046672 ) ) ;
#5068 = ADVANCED_FACE ( 'NONE', ( #7830 ), #4975, .T. ) ;
#5069 = FACE_OUTER_BOUND ( 'NONE', #743, .T. ) ;
#5070 = CARTESIAN_POINT ( 'NONE',  ( -2.625000000000000444, -27.79166666666666430, -4.546633369868303021 ) ) ;
#5071 = CARTESIAN_POINT ( 'NONE',  ( -5.114683531250000748, -29.54687500034139802, -6.263680815196995234E-16 ) ) ;
#5072 = CARTESIAN_POINT ( 'NONE',  ( -2.462045979635576920, -3.249340926099361315, -2.487701488670255756 ) ) ;
#5073 = ORIENTED_EDGE ( 'NONE', *, *, #3505, .T. ) ;
#5074 = CARTESIAN_POINT ( 'NONE',  ( 5.250000000000000000, -28.06249999931720396, -6.429395695523604153E-16 ) ) ;
#5075 = CARTESIAN_POINT ( 'NONE',  ( 0.000000000000000000, 76.00000000000000000, 0.000000000000000000 ) ) ;
#5076 = CARTESIAN_POINT ( 'NONE',  ( -2.557341765625002594, -28.69270833367473017, 4.429445870380399164 ) ) ;
#5077 =( BOUNDED_CURVE ( )  B_SPLINE_CURVE ( 2, ( #1788, #382, #8109, #5356, #4574, #8204, #6802, #7550, #8934 ),
 .UNSPECIFIED., .F., .T. ) 
 B_SPLINE_CURVE_WITH_KNOTS ( ( 3, 2, 2, 2, 3 ),
 ( 0.6041666666666666297, 0.6111111111111111605, 0.6250000000000000000, 0.6388888888888888395, 0.6458333333333333703 ),
 .UNSPECIFIED. ) 
 CURVE ( )  GEOMETRIC_REPRESENTATION_ITEM ( )  RATIONAL_B_SPLINE_CURVE ( ( 0.9330127018922192983, 0.9330127018922187432, 1.000000000000000000, 0.8660254037844387076, 1.000000000000000000, 0.8660254037844387076, 1.000000000000000000, 0.9330127018922187432, 0.9330127018922192983 ) ) 
 REPRESENTATION_ITEM ( '' )  );
#5078 = ORIENTED_EDGE ( 'NONE', *, *, #7298, .T. ) ;
#5079 = EDGE_LOOP ( 'NONE', ( #5622, #3845 ) ) ;
#5080 = FACE_OUTER_BOUND ( 'NONE', #3852, .T. ) ;
#5081 = EDGE_CURVE ( 'NONE', #1056, #8090, #7028, .T. ) ;
#5082 = CARTESIAN_POINT ( 'NONE',  ( 1.142306659890740623E-15, -28.04687499965860198, 6.218427825808274356 ) ) ;
#5083 = CARTESIAN_POINT ( 'NONE',  ( 3.992485675378568910, -2.250659073900638685, -1.674995433905514863 ) ) ;
#5084 = AXIS2_PLACEMENT_3D ( 'NONE', #5639, #3051, #5868 ) ;
#5085 = CARTESIAN_POINT ( 'NONE',  ( 5.143405491005359555E-16, -28.00000000000000000, 4.199909308207393721 ) ) ;
#5086 = AXIS2_PLACEMENT_3D ( 'NONE', #7147, #7848, #9100 ) ;
#5087 = ORIENTED_EDGE ( 'NONE', *, *, #761, .T. ) ;
#5088 = CARTESIAN_POINT ( 'NONE',  ( -5.249999999999999112, -27.95833333265052900, -3.031088913245534755 ) ) ;
#5089 = VECTOR ( 'NONE', #2367, 1000.000000000000000 ) ;
#5090 = CARTESIAN_POINT ( 'NONE',  ( 5.250000000000000000, -29.53125000068279604, 0.000000000000000000 ) ) ;
#5091 = CARTESIAN_POINT ( 'NONE',  ( 1.142306659890740623E-15, -28.04687499965860198, 6.218427825808274356 ) ) ;
#5092 = AXIS2_PLACEMENT_3D ( 'NONE', #7876, #1495, #6465 ) ;
#5093 = CARTESIAN_POINT ( 'NONE',  ( -5.114683531250000748, -26.98437500034139802, -6.263680815196995234E-16 ) ) ;
#5094 = CYLINDRICAL_SURFACE ( 'NONE', #6574, 5.250000000000000000 ) ;
#5095 = CARTESIAN_POINT ( 'NONE',  ( 2.161402558328724325E-14, -28.99999999931720751, -5.250000000000000000 ) ) ;
#5096 = CARTESIAN_POINT ( 'NONE',  ( 2.108492589042352705, -3.950659073900640195, -2.134148098076933397 ) ) ;
#5097 = CARTESIAN_POINT ( 'NONE',  ( 0.000000000000000000, -27.00000000000000000, 0.000000000000000000 ) ) ;
#5098 = CARTESIAN_POINT ( 'NONE',  ( 4.000000000000000000, -2.649340926099360782, 0.01814118441321914063 ) ) ;
#5099 = CARTESIAN_POINT ( 'NONE',  ( -5.250000000000000000, -27.45833333265053611, -3.031088913245534755 ) ) ;
#5100 = DIRECTION ( 'NONE',  ( 0.000000000000000000, 1.000000000000000000, 0.000000000000000000 ) ) ;
#5101 = FACE_OUTER_BOUND ( 'NONE', #4794, .T. ) ;
#5102 = CARTESIAN_POINT ( 'NONE',  ( 0.000000000000000000, -20.00000000000000000, -3.500000000000000444 ) ) ;
#5103 = VERTEX_POINT ( 'NONE', #798 ) ;
#5104 =( LENGTH_UNIT ( ) NAMED_UNIT ( * ) SI_UNIT ( .MILLI., .METRE. ) );
#5105 = CARTESIAN_POINT ( 'NONE',  ( -2.692658234374996518, -27.53645833299193413, 4.663820869356208654 ) ) ;
#5106 = LINE ( 'NONE', #1317, #5764 ) ;
#5107 = ORIENTED_EDGE ( 'NONE', *, *, #4861, .T. ) ;
#5108 = CARTESIAN_POINT ( 'NONE',  ( 1.142306659890740623E-15, -27.26562499965860553, 6.218427825808274356 ) ) ;
#5109 = CARTESIAN_POINT ( 'NONE',  ( 2.134148098076933397, -6.750659073900640017, 2.108492589042352261 ) ) ;
#5110 = ORIENTED_EDGE ( 'NONE', *, *, #4698, .F. ) ;
#5111 = CARTESIAN_POINT ( 'NONE',  ( -5.250000000000000000, -29.14583333333333925, -3.031088913245536531 ) ) ;
#5112 = EDGE_CURVE ( 'NONE', #6553, #7820, #3642, .T. ) ;
#5113 = CARTESIAN_POINT ( 'NONE',  ( -5.114683531250001636, -27.27604166700806587, 2.952963913586931444 ) ) ;
#5114 = CARTESIAN_POINT ( 'NONE',  ( 5.250000000000000000, -27.35416666666666430, -3.031088913245536531 ) ) ;
#5115 = PRODUCT_DEFINITION ( 'UNKNOWN', '', #2191, #7012 ) ;
#5116 = LINE ( 'NONE', #7963, #4645 ) ;
#5117 = CARTESIAN_POINT ( 'NONE',  ( -1.431606283892620235, -6.349340926099360516, -3.507514324621463953 ) ) ;
#5118 = CARTESIAN_POINT ( 'NONE',  ( 8.603239422292019767E-08, -29.99999999999999645, -5.249999999999998224 ) ) ;
#5119 = CARTESIAN_POINT ( 'NONE',  ( 1.406733260263397289, -28.80133545031537423, 5.249999999999997335 ) ) ;
#5120 = CARTESIAN_POINT ( 'NONE',  ( -5.114683531249999859, -29.81770833367473017, -2.952963913586935440 ) ) ;
#5121 = CARTESIAN_POINT ( 'NONE',  ( 2.624999999999996891, -28.32291666734946389, 4.546633369868304797 ) ) ;
#5122 = ORIENTED_EDGE ( 'NONE', *, *, #6771, .F. ) ;
#5123 = CARTESIAN_POINT ( 'NONE',  ( 0.000000000000000000, 81.00000000000001421, 0.000000000000000000 ) ) ;
#5124 = CARTESIAN_POINT ( 'NONE',  ( 2.033577675846918216E-14, -28.06249999999999645, 5.250000000000000888 ) ) ;
#5125 = CARTESIAN_POINT ( 'NONE',  ( -2.557341765625002594, -28.44270833367473017, 4.429445870380399164 ) ) ;
#5126 = ORIENTED_EDGE ( 'NONE', *, *, #3522, .F. ) ;
#5127 = CARTESIAN_POINT ( 'NONE',  ( 0.000000000000000000, -27.00000000000000000, -6.250000000000000000 ) ) ;
#5128 = CARTESIAN_POINT ( 'NONE',  ( 1.142306659890740623E-15, -27.79687499965860198, 6.218427825808274356 ) ) ;
#5129 = CARTESIAN_POINT ( 'NONE',  ( 2.841254879263473310, -5.150659073900639484, 2.815599370228907272 ) ) ;
#5130 = ADVANCED_FACE ( 'NONE', ( #4849 ), #2950, .T. ) ;
#5131 = CARTESIAN_POINT ( 'NONE',  ( 5.249999999999999112, -29.29166666598386826, -3.031088913245536975 ) ) ;
#5132 = EDGE_LOOP ( 'NONE', ( #372, #3900, #8266, #7731 ) ) ;
#5133 = MANIFOLD_SOLID_BREP ( 'Cut-Extrude-Thin1', #2686 ) ;
#5134 =( BOUNDED_CURVE ( )  B_SPLINE_CURVE ( 2, ( #5663, #38, #4916, #8592, #7854, #2092, #1347, #7812, #7018 ),
 .UNSPECIFIED., .F., .F. ) 
 B_SPLINE_CURVE_WITH_KNOTS ( ( 3, 2, 2, 2, 3 ),
 ( 0.5208333333333333703, 0.5277777777777777901, 0.5416666666666666297, 0.5555555555555555802, 0.5625000000000000000 ),
 .UNSPECIFIED. ) 
 CURVE ( )  GEOMETRIC_REPRESENTATION_ITEM ( )  RATIONAL_B_SPLINE_CURVE ( ( 0.9330127018922192983, 0.9330127018922198534, 1.000000000000000000, 0.8660254037844387076, 1.000000000000000000, 0.8660254037844387076, 1.000000000000000000, 0.9330127018922194093, 0.9330127018922194093 ) ) 
 REPRESENTATION_ITEM ( '' )  );
#5135 = ADVANCED_FACE ( 'NONE', ( #7969 ), #7925, .F. ) ;
#5136 = CARTESIAN_POINT ( 'NONE',  ( -6.972266317189433020E-16, -29.81250000000000000, -5.250000000000000000 ) ) ;
#5137 = CARTESIAN_POINT ( 'NONE',  ( -2.625000000000002220, -29.36458333401613174, 4.546633369868302132 ) ) ;
#5138 = CARTESIAN_POINT ( 'NONE',  ( 2.692658234375002735, -28.52604166632526628, 4.663820869356205101 ) ) ;
#5139 = CARTESIAN_POINT ( 'NONE',  ( -2.557341765624999042, -29.83854166700806232, -4.429445870380400052 ) ) ;
#5140 = CARTESIAN_POINT ( 'NONE',  ( 1.431606283892619125, -2.349340926099361848, 3.507514324621464397 ) ) ;
#5141 = CARTESIAN_POINT ( 'NONE',  ( 2.692658234374998738, -27.41145833299193413, -4.663820869356206877 ) ) ;
#5142 = EDGE_CURVE ( 'NONE', #5957, #5960, #3180, .T. ) ;
#5143 = CARTESIAN_POINT ( 'NONE',  ( -1.224499502706140497, -0.05065907390063940224, 3.007514324621436863 ) ) ;
#5144 = UNCERTAINTY_MEASURE_WITH_UNIT (LENGTH_MEASURE( 1.000000000000000082E-05 ), #5512, 'distance_accuracy_value', 'NONE');
#5145 = DIRECTION ( 'NONE',  ( 0.000000000000000000, 0.000000000000000000, -1.000000000000000000 ) ) ;
#5146 = CARTESIAN_POINT ( 'NONE',  ( 2.841254879263533262, -4.449340926099361937, -2.815599370228847320 ) ) ;
#5147 = CARTESIAN_POINT ( 'NONE',  ( -5.249999999999999112, -27.41666666598386826, 3.031088913245538308 ) ) ;
#5148 = DIRECTION ( 'NONE',  ( 0.000000000000000000, 0.000000000000000000, -1.000000000000000000 ) ) ;
#5149 = DIRECTION ( 'NONE',  ( 0.000000000000000000, -1.000000000000000000, 0.000000000000000000 ) ) ;
#5150 = DIRECTION ( 'NONE',  ( 0.000000000000000000, 0.000000000000000000, -1.000000000000000000 ) ) ;
#5151 = ORIENTED_EDGE ( 'NONE', *, *, #924, .T. ) ;
#5152 = CARTESIAN_POINT ( 'NONE',  ( 0.000000000000000000, 0.000000000000000000, 0.000000000000000000 ) ) ;
#5153 = CARTESIAN_POINT ( 'NONE',  ( 1.142306659890740623E-15, -28.51562499965860198, 6.218427825808274356 ) ) ;
#5154 = CARTESIAN_POINT ( 'NONE',  ( 0.01814118441321938349, -3.049340926099361138, -4.000000000000000000 ) ) ;
#5155 = CARTESIAN_POINT ( 'NONE',  ( 0.000000000000000000, -27.00000000000000000, 0.000000000000000000 ) ) ;
#5156 = ORIENTED_EDGE ( 'NONE', *, *, #3316, .F. ) ;
#5157 = CARTESIAN_POINT ( 'NONE',  ( -5.250000000000000000, -27.25000000000000000, 0.000000000000000000 ) ) ;
#5158 = EDGE_CURVE ( 'NONE', #3172, #3585, #3308, .T. ) ;
#5159 = CARTESIAN_POINT ( 'NONE',  ( 0.01814118441314514080, -6.550659073900640728, 3.000000000000000444 ) ) ;
#5160 = ORIENTED_EDGE ( 'NONE', *, *, #8722, .F. ) ;
#5161 = CARTESIAN_POINT ( 'NONE',  ( -5.250000000000000000, -27.37500000000000000, -6.429395695523604153E-16 ) ) ;
#5162 = ADVANCED_FACE ( 'NONE', ( #1644 ), #2440, .F. ) ;
#5163 = CARTESIAN_POINT ( 'NONE',  ( -2.557341765624999042, -27.83854166700806587, -4.429445870380400052 ) ) ;
#5164 = ADVANCED_FACE ( 'NONE', ( #4577 ), #1593, .F. ) ;
#5165 = CARTESIAN_POINT ( 'NONE',  ( 5.250000000000000000, -27.37500000000000000, -6.429395695523604153E-16 ) ) ;
#5166 = CARTESIAN_POINT ( 'NONE',  ( 0.000000000000000000, -30.00000000000000000, 5.250000000000000000 ) ) ;
#5167 = CARTESIAN_POINT ( 'NONE',  ( -3.507514324621464397, -5.149340926099360338, 1.431606283892619347 ) ) ;
#5168 = CARTESIAN_POINT ( 'NONE',  ( -5.249999999999999112, -29.95833333265053255, -3.031088913245534755 ) ) ;
#5169 = CARTESIAN_POINT ( 'NONE',  ( -5.250000000000000000, -27.40625000068279604, -6.429395695523604153E-16 ) ) ;
#5170 = CARTESIAN_POINT ( 'NONE',  ( -5.114683531249999859, -29.06770833367473017, -2.952963913586935440 ) ) ;
#5171 = CARTESIAN_POINT ( 'NONE',  ( 5.250000000000000000, -28.28125000068279604, 0.000000000000000000 ) ) ;
#5172 = VERTEX_POINT ( 'NONE', #7412 ) ;
#5173 = DIRECTION ( 'NONE',  ( 0.000000000000000000, 0.9973637043974448169, 0.07256473765270717025 ) ) ;
#5174 = DIRECTION ( 'NONE',  ( 0.000000000000000000, -1.000000000000000000, 0.000000000000000000 ) ) ;
#5175 = CARTESIAN_POINT ( 'NONE',  ( 2.557341765625000818, -27.81770833367473017, -4.429445870380400052 ) ) ;
#5176 = AXIS2_PLACEMENT_3D ( 'NONE', #3728, #5204, #4606 ) ;
#5177 = ORIENTED_EDGE ( 'NONE', *, *, #2414, .F. ) ;
#5178 = CARTESIAN_POINT ( 'NONE',  ( 1.406733260263402174, -26.83258545099816672, 5.249999999999995559 ) ) ;
#5179 = CARTESIAN_POINT ( 'NONE',  ( -5.385316468750001029, -28.13020833299193058, -3.109213912904136734 ) ) ;
#5180 = CARTESIAN_POINT ( 'NONE',  ( 4.000000000000000000, -3.750659073900638685, -0.01814118441313441674 ) ) ;
#5181 = DIRECTION ( 'NONE',  ( 0.000000000000000000, 0.000000000000000000, -1.000000000000000000 ) ) ;
#5182 = VECTOR ( 'NONE', #1904, 1000.000000000000000 ) ;
#5183 = ORIENTED_EDGE ( 'NONE', *, *, #5647, .F. ) ;
#5184 = CARTESIAN_POINT ( 'NONE',  ( 6.972266317189433020E-16, -29.71875000068279249, -5.249999999999999112 ) ) ;
#5185 = CARTESIAN_POINT ( 'NONE',  ( 5.250000000000000000, -29.01041666734946389, -3.031088913245534755 ) ) ;
#5186 = CARTESIAN_POINT ( 'NONE',  ( -3.807688866302469071E-16, -28.17187499965860553, -6.218427825808274356 ) ) ;
#5187 = VECTOR ( 'NONE', #5367, 1000.000000000000000 ) ;
#5188 = CARTESIAN_POINT ( 'NONE',  ( -1.084901341431563923E-15, -29.73437500034140157, 5.905927827173866440 ) ) ;
#5189 = ORIENTED_EDGE ( 'NONE', *, *, #609, .T. ) ;
#5190 = CARTESIAN_POINT ( 'NONE',  ( -3.807688866302469071E-16, -27.39062499965860198, -6.218427825808274356 ) ) ;
#5191 = CARTESIAN_POINT ( 'NONE',  ( 0.01814118441320878086, -7.849340926099363180, -3.000000000000000444 ) ) ;
#5192 = AXIS2_PLACEMENT_3D ( 'NONE', #7003, #8445, #3515 ) ;
#5193 = CARTESIAN_POINT ( 'NONE',  ( 0.000000000000000000, -30.00000000000000000, 0.000000000000000000 ) ) ;
#5194 = CARTESIAN_POINT ( 'NONE',  ( 0.01814118441321938349, -3.049340926099361138, -4.000000000000000000 ) ) ;
#5195 = EDGE_CURVE ( 'NONE', #5024, #8201, #7326, .T. ) ;
#5196 = CARTESIAN_POINT ( 'NONE',  ( 5.250000000000000888, -27.58333333265053966, 3.031088913245532979 ) ) ;
#5197 = LINE ( 'NONE', #2699, #7034 ) ;
#5198 = CARTESIAN_POINT ( 'NONE',  ( 3.492485675378535603, -0.9493409260993610488, 1.467888652719046672 ) ) ;
#5199 = AXIS2_PLACEMENT_3D ( 'NONE', #8504, #4179, #1469 ) ;
#5200 = CARTESIAN_POINT ( 'NONE',  ( 1.406733260263403507, -29.76116454900183328, -5.249999999999994671 ) ) ;
#5201 = DIRECTION ( 'NONE',  ( 1.000000000000000000, 0.000000000000000000, 0.000000000000000000 ) ) ;
#5202 = CARTESIAN_POINT ( 'NONE',  ( -5.385316468749998364, -27.80729166632526628, 3.109213912904140287 ) ) ;
#5203 = CARTESIAN_POINT ( 'NONE',  ( -1.638713065079163034, -4.749340926099361759, -4.007514324621466173 ) ) ;
#5204 = DIRECTION ( 'NONE',  ( 0.000000000000000000, 1.000000000000000000, 0.000000000000000000 ) ) ;
#5205 = ORIENTED_EDGE ( 'NONE', *, *, #3479, .T. ) ;
#5206 = CARTESIAN_POINT ( 'NONE',  ( 5.385316468749999252, -27.93229166632526628, -3.109213912904139399 ) ) ;
#5207 = CARTESIAN_POINT ( 'NONE',  ( -3.000000000000000444, -7.750659073900639129, 0.01814118441314532468 ) ) ;
#5208 = CONICAL_SURFACE ( 'NONE', #7288, 3.500000000000000444, 0.08726646259971666819 ) ;
#5209 = ORIENTED_EDGE ( 'NONE', *, *, #3316, .T. ) ;
#5210 = CARTESIAN_POINT ( 'NONE',  ( 5.249999999999999112, -28.27083333333332860, 3.031088913245538308 ) ) ;
#5211 = CARTESIAN_POINT ( 'NONE',  ( 2.557341765625000818, -27.88020833367473017, -4.429445870380400052 ) ) ;
#5212 = PRESENTATION_STYLE_ASSIGNMENT (( #6749 ) ) ;
#5213 = CARTESIAN_POINT ( 'NONE',  ( -5.250000000000000888, -29.38541666734946034, 3.031088913245533423 ) ) ;
#5214 = MANIFOLD_SOLID_BREP ( 'Thread1', #7124 ) ;
#5215 = CARTESIAN_POINT ( 'NONE',  ( -2.624999999999996891, -30.14583333265053611, 4.546633369868304797 ) ) ;
#5216 = CARTESIAN_POINT ( 'NONE',  ( -0.01814118441321365544, -0.6493409260993610044, 3.500000000000000000 ) ) ;
#5217 = CARTESIAN_POINT ( 'NONE',  ( 5.250000000000000000, -28.78125000068279604, 0.000000000000000000 ) ) ;
#5218 = LINE ( 'NONE', #287, #494 ) ;
#5219 = CARTESIAN_POINT ( 'NONE',  ( -2.557341765624999042, -28.83854166700806587, -4.429445870380400052 ) ) ;
#5220 =( BOUNDED_CURVE ( )  B_SPLINE_CURVE ( 2, ( #1455, #6339, #6299, #7749, #4122, #2070, #5644, #4300, #1414 ),
 .UNSPECIFIED., .F., .T. ) 
 B_SPLINE_CURVE_WITH_KNOTS ( ( 3, 2, 2, 2, 3 ),
 ( 0.8125000000000000000, 0.8194444444444444198, 0.8333333333333333703, 0.8472222222222222099, 0.8541666666666667407 ),
 .UNSPECIFIED. ) 
 CURVE ( )  GEOMETRIC_REPRESENTATION_ITEM ( )  RATIONAL_B_SPLINE_CURVE ( ( 0.9330127018922194093, 0.9330127018922194093, 1.000000000000000000, 0.8660254037844387076, 1.000000000000000000, 0.8660254037844387076, 1.000000000000000000, 0.9330127018922187432, 0.9330127018922192983 ) ) 
 REPRESENTATION_ITEM ( '' )  );
#5221 = VERTEX_POINT ( 'NONE', #6659 ) ;
#5222 = FACE_OUTER_BOUND ( 'NONE', #3084, .T. ) ;
#5223 = CARTESIAN_POINT ( 'NONE',  ( 2.557341765625000818, -29.06770833367473017, -4.429445870380400052 ) ) ;
#5224 = EDGE_LOOP ( 'NONE', ( #7973, #714, #2421, #3677, #8977, #710 ) ) ;
#5225 = DIRECTION ( 'NONE',  ( 0.000000000000000000, 0.000000000000000000, -1.000000000000000000 ) ) ;
#5226 = CARTESIAN_POINT ( 'NONE',  ( 2.692658234374998738, -27.44270833299193413, -4.663820869356206877 ) ) ;
#5227 = CARTESIAN_POINT ( 'NONE',  ( -4.007514324621431534, -4.450659073900638418, -1.638713065079248521 ) ) ;
#5228 = SURFACE_SIDE_STYLE ('',( #2964 ) ) ;
#5229 = CARTESIAN_POINT ( 'NONE',  ( 2.692658234374998738, -27.94270833299193413, -4.663820869356206877 ) ) ;
#5230 = ORIENTED_EDGE ( 'NONE', *, *, #1496, .T. ) ;
#5231 = CARTESIAN_POINT ( 'NONE',  ( -5.250000000000000000, -29.87500000000000000, -6.429395695523604153E-16 ) ) ;
#5232 = CARTESIAN_POINT ( 'NONE',  ( 5.250000000000000000, -28.78125000068279604, 0.000000000000000000 ) ) ;
#5233 = EDGE_CURVE ( 'NONE', #5696, #4680, #331, .T. ) ;
#5234 = CARTESIAN_POINT ( 'NONE',  ( 5.385316468750001029, -28.00520833299193413, 3.109213912904135846 ) ) ;
#5235 = CARTESIAN_POINT ( 'NONE',  ( 3.616337804771879580E-16, -27.04687500034139802, -5.905927827173866440 ) ) ;
#5236 = EDGE_LOOP ( 'NONE', ( #8105, #4578, #5814, #832 ) ) ;
#5237 = DIRECTION ( 'NONE',  ( 0.000000000000000000, 1.000000000000000000, 0.000000000000000000 ) ) ;
#5238 = CARTESIAN_POINT ( 'NONE',  ( 2.992485675378565357, -5.450659073900638418, -1.260781871532430376 ) ) ;
#5239 = LINE ( 'NONE', #5285, #1325 ) ;
#5240 = AXIS2_PLACEMENT_3D ( 'NONE', #8136, #6544, #266 ) ;
#5241 = CONICAL_SURFACE ( 'NONE', #1840, 6.250000000000002665, 0.1221730476396033355 ) ;
#5242 = CARTESIAN_POINT ( 'NONE',  ( 2.624999999999998668, -28.52083333265053611, -4.546633369868303021 ) ) ;
#5243 = DIRECTION ( 'NONE',  ( 0.000000000000000000, -1.000000000000000000, 0.000000000000000000 ) ) ;
#5244 = CARTESIAN_POINT ( 'NONE',  ( -2.462045979635576920, -1.649340926099361004, -2.487701488670255756 ) ) ;
#5245 = CARTESIAN_POINT ( 'NONE',  ( 5.249999999999999112, -29.54166666598386470, -3.031088913245536975 ) ) ;
#5246 = CARTESIAN_POINT ( 'NONE',  ( 0.000000000000000000, -30.00000000000000000, 0.000000000000000000 ) ) ;
#5247 = DIRECTION ( 'NONE',  ( 1.000000000000000000, 0.000000000000000000, 0.000000000000000000 ) ) ;
#5248 = CARTESIAN_POINT ( 'NONE',  ( -5.385316468750000141, -27.82812499965860198, 0.000000000000000000 ) ) ;
#5249 = CARTESIAN_POINT ( 'NONE',  ( 4.007514324621469726, -7.549340926099361582, -1.638713065079161257 ) ) ;
#5250 = CARTESIAN_POINT ( 'NONE',  ( 1.000000000000000000, -29.00000000000000355, 2.431755684948965435 ) ) ;
#5251 = ORIENTED_EDGE ( 'NONE', *, *, #4302, .F. ) ;
#5252 = CARTESIAN_POINT ( 'NONE',  ( -2.692658234375000514, -28.86979166632526983, -4.663820869356205989 ) ) ;
#5253 = CARTESIAN_POINT ( 'NONE',  ( -2.487701488670202910, -1.150659073900638818, -2.462045979635629767 ) ) ;
#5254 = EDGE_LOOP ( 'NONE', ( #1793, #856, #1, #4325 ) ) ;
#5255 = CARTESIAN_POINT ( 'NONE',  ( -1.113604000661152470E-15, -28.31250000000000000, 6.062177826491070398 ) ) ;
#5256 = CARTESIAN_POINT ( 'NONE',  ( 3.500000000000000000, -0.5506590739006389512, -0.01814118441313969030 ) ) ;
#5257 = EDGE_LOOP ( 'NONE', ( #91, #988, #7364, #1826 ) ) ;
#5258 = CARTESIAN_POINT ( 'NONE',  ( -2.625000000000000444, -27.29166666666666430, -4.546633369868303021 ) ) ;
#5259 = VERTEX_POINT ( 'NONE', #8206 ) ;
#5260 = EDGE_CURVE ( 'NONE', #1166, #1171, #6055, .T. ) ;
#5261 = CARTESIAN_POINT ( 'NONE',  ( -5.114683531250001636, -28.46354166700806587, 2.952963913586931444 ) ) ;
#5262 = CARTESIAN_POINT ( 'NONE',  ( -2.462045979635576920, -1.649340926099361004, -2.487701488670255756 ) ) ;
#5263 = CARTESIAN_POINT ( 'NONE',  ( 0.000000000000000000, -20.00000000000000000, 0.000000000000000000 ) ) ;
#5264 = CARTESIAN_POINT ( 'NONE',  ( 0.000000000000000000, -27.00000000000000000, 0.000000000000000000 ) ) ;
#5265 = CARTESIAN_POINT ( 'NONE',  ( 5.114683531250000748, -28.92187500034139802, 0.000000000000000000 ) ) ;
#5266 =( LENGTH_UNIT ( ) NAMED_UNIT ( * ) SI_UNIT ( .MILLI., .METRE. ) );
#5267 = ORIENTED_EDGE ( 'NONE', *, *, #2369, .F. ) ;
#5268 = CARTESIAN_POINT ( 'NONE',  ( -1.975475456537005874E-15, -29.31250000000000000, 5.250000000000000000 ) ) ;
#5269 = CARTESIAN_POINT ( 'NONE',  ( 5.114683531249998971, -27.13020833367473372, 2.952963913586936329 ) ) ;
#5270 = APPLICATION_CONTEXT ( 'automotive_design' ) ;
#5271 = EDGE_LOOP ( 'NONE', ( #5362, #8247, #1897, #8896 ) ) ;
#5272 =( BOUNDED_CURVE ( )  B_SPLINE_CURVE ( 2, ( #3616, #5042, #1424, #8634, #4910, #6441, #4864, #680, #638 ),
 .UNSPECIFIED., .F., .T. ) 
 B_SPLINE_CURVE_WITH_KNOTS ( ( 3, 2, 2, 2, 3 ),
 ( 0.6458333333333333703, 0.6527777777777777901, 0.6666666666666666297, 0.6805555555555555802, 0.6875000000000000000 ),
 .UNSPECIFIED. ) 
 CURVE ( )  GEOMETRIC_REPRESENTATION_ITEM ( )  RATIONAL_B_SPLINE_CURVE ( ( 0.9330127018922192983, 0.9330127018922198534, 1.000000000000000000, 0.8660254037844387076, 1.000000000000000000, 0.8660254037844387076, 1.000000000000000000, 0.9330127018922194093, 0.9330127018922194093 ) ) 
 REPRESENTATION_ITEM ( '' )  );
#5273 = CARTESIAN_POINT ( 'NONE',  ( -5.385316468750000141, -27.10937499965860198, 0.000000000000000000 ) ) ;
#5274 = CARTESIAN_POINT ( 'NONE',  ( -5.385316468750001029, -28.88020833299193058, -3.109213912904136734 ) ) ;
#5275 = CARTESIAN_POINT ( 'NONE',  ( 4.000000000000000000, -6.950659073900639306, -0.01814118441313441674 ) ) ;
#5276 = CARTESIAN_POINT ( 'NONE',  ( 1.185285273922203525E-14, -29.18750000000000000, -5.250000000000000000 ) ) ;
#5277 = CARTESIAN_POINT ( 'NONE',  ( -5.385316468750001029, -27.63020833299193413, -3.109213912904136734 ) ) ;
#5278 = ORIENTED_EDGE ( 'NONE', *, *, #1228, .T. ) ;
#5279 = CARTESIAN_POINT ( 'NONE',  ( 5.250000000000000888, -29.89583333333333215, 3.031088913245533423 ) ) ;
#5280 = CARTESIAN_POINT ( 'NONE',  ( -5.250000000000000000, -29.67708333401613174, -3.031088913245536531 ) ) ;
#5281 = CARTESIAN_POINT ( 'NONE',  ( -5.385316468749998364, -27.33854166632526628, 3.109213912904140287 ) ) ;
#5282 = VERTEX_POINT ( 'NONE', #6246 ) ;
#5283 = CARTESIAN_POINT ( 'NONE',  ( -3.807688866302469071E-16, -28.64062499965860198, -6.218427825808274356 ) ) ;
#5284 = CARTESIAN_POINT ( 'NONE',  ( -2.108492589042352261, 0.04934092609936062412, 2.134148098076933397 ) ) ;
#5285 = CARTESIAN_POINT ( 'NONE',  ( 0.000000000000000000, -30.00000000000000000, 5.250000000000000000 ) ) ;
#5286 = CARTESIAN_POINT ( 'NONE',  ( 2.625000000000002220, -27.60416666598386826, 4.546633369868302132 ) ) ;
#5287 = DIRECTION ( 'NONE',  ( 0.000000000000000000, 0.000000000000000000, -1.000000000000000000 ) ) ;
#5288 = CARTESIAN_POINT ( 'NONE',  ( -2.487701488670255312, -2.049340926099361582, 2.462045979635577808 ) ) ;
#5289 = CARTESIAN_POINT ( 'NONE',  ( 0.000000000000000000, 76.00000000000000000, -2.499999999999999556 ) ) ;
#5290 = ORIENTED_EDGE ( 'NONE', *, *, #7150, .F. ) ;
#5291 = CARTESIAN_POINT ( 'NONE',  ( 5.385316468750000141, -28.70312499965860198, -6.595110575850215044E-16 ) ) ;
#5292 = CARTESIAN_POINT ( 'NONE',  ( -1.638713065079163034, -6.349340926099361404, -4.007514324621466173 ) ) ;
#5293 = CARTESIAN_POINT ( 'NONE',  ( -2.625000000000002220, -29.58333333333333215, 4.546633369868302132 ) ) ;
#5294 = ORIENTED_EDGE ( 'NONE', *, *, #3331, .F. ) ;
#5295 = CARTESIAN_POINT ( 'NONE',  ( -2.692658234375000514, -27.86979166632526628, -4.663820869356205989 ) ) ;
#5296 = CARTESIAN_POINT ( 'NONE',  ( -2.462045979635629323, -6.350659073900638774, 2.487701488670203798 ) ) ;
#5297 = ORIENTED_EDGE ( 'NONE', *, *, #1915, .F. ) ;
#5298 = CARTESIAN_POINT ( 'NONE',  ( -2.625000000000002220, -28.08333333333333215, 4.546633369868302132 ) ) ;
#5299 = CARTESIAN_POINT ( 'NONE',  ( -3.500000000000000000, -1.350659073900638996, 0.01814118441314012051 ) ) ;
#5300 = EDGE_CURVE ( 'NONE', #2431, #2212, #6030, .T. ) ;
#5301 = ORIENTED_EDGE ( 'NONE', *, *, #7310, .F. ) ;
#5302 = CARTESIAN_POINT ( 'NONE',  ( 5.250000000000000000, -27.10416666666666430, -3.031088913245536531 ) ) ;
#5303 = EDGE_LOOP ( 'NONE', ( #2160, #673, #135, #5160 ) ) ;
#5304 = CARTESIAN_POINT ( 'NONE',  ( -1.084901341431563726E-15, -28.42187500034139802, 5.905927827173866440 ) ) ;
#5305 = ADVANCED_FACE ( 'NONE', ( #1931, #1088 ), #4067, .F. ) ;
#5306 = CARTESIAN_POINT ( 'NONE',  ( -1.224499502706077880, -1.549340926099361804, -3.007514324621463064 ) ) ;
#5307 = CARTESIAN_POINT ( 'NONE',  ( 2.624999999999996891, -28.57291666734946389, 4.546633369868304797 ) ) ;
#5308 = CARTESIAN_POINT ( 'NONE',  ( 5.114683531249999859, -28.15104166700806587, -2.952963913586932776 ) ) ;
#5309 = CARTESIAN_POINT ( 'NONE',  ( 5.249999999999999112, -27.26041666734946034, -3.031088913245534755 ) ) ;
#5310 = EDGE_CURVE ( 'NONE', #2524, #3224, #85, .T. ) ;
#5311 = CARTESIAN_POINT ( 'NONE',  ( -1.930746022523279315, -1.460316824068202362E-13, 2.881131468811274576 ) ) ;
#5312 = CARTESIAN_POINT ( 'NONE',  ( 5.114683531249998971, -27.38020833367473017, 2.952963913586936329 ) ) ;
#5313 = ORIENTED_EDGE ( 'NONE', *, *, #7954, .T. ) ;
#5314 = DIRECTION ( 'NONE',  ( 0.000000000000000000, 1.000000000000000000, 0.000000000000000000 ) ) ;
#5315 = CARTESIAN_POINT ( 'NONE',  ( -3.807688866302469071E-16, -29.42187499965860198, -6.218427825808274356 ) ) ;
#5316 = CYLINDRICAL_SURFACE ( 'NONE', #3709, 5.250000000000000000 ) ;
#5317 = CARTESIAN_POINT ( 'NONE',  ( 2.692658234374998738, -29.69270833299193413, -4.663820869356206877 ) ) ;
#5318 = VECTOR ( 'NONE', #7711, 1000.000000000000000 ) ;
#5319 = ORIENTED_EDGE ( 'NONE', *, *, #1403, .T. ) ;
#5320 = AXIS2_PLACEMENT_3D ( 'NONE', #4764, #1094, #341 ) ;
#5321 = FACE_OUTER_BOUND ( 'NONE', #2376, .T. ) ;
#5322 = CARTESIAN_POINT ( 'NONE',  ( 3.712013335537174572E-16, -27.96875000068279604, -6.062177826491070398 ) ) ;
#5323 = CARTESIAN_POINT ( 'NONE',  ( 5.385316468750000141, -29.48437499965859843, -6.595110575850215044E-16 ) ) ;
#5324 = EDGE_LOOP ( 'NONE', ( #2323, #4490 ) ) ;
#5325 = CIRCLE ( 'NONE', #1933, 4.250000000000000000 ) ;
#5326 = CARTESIAN_POINT ( 'NONE',  ( -5.385316468750000141, -28.82812499965860198, 0.000000000000000000 ) ) ;
#5327 = CARTESIAN_POINT ( 'NONE',  ( -3.007514324621435531, -7.650659073900639484, -1.224499502706142273 ) ) ;
#5328 = CARTESIAN_POINT ( 'NONE',  ( 2.625000000000000444, -29.45833333333333215, -4.546633369868303021 ) ) ;
#5329 = PRODUCT_DEFINITION_SHAPE ( 'NONE', 'NONE',  #4331 ) ;
#5330 = ADVANCED_FACE ( 'NONE', ( #572, #2585 ), #9031, .T. ) ;
#5331 = ADVANCED_FACE ( 'NONE', ( #7603 ), #4713, .T. ) ;
#5332 = CARTESIAN_POINT ( 'NONE',  ( 0.000000000000000000, -9.000000000000000000, 0.000000000000000000 ) ) ;
#5333 = DIRECTION ( 'NONE',  ( 0.000000000000000000, 0.000000000000000000, -1.000000000000000000 ) ) ;
#5334 = COLOUR_RGB ( '',0.8941176470588234615, 0.8941176470588234615, 0.8941176470588234615 ) ;
#5335 = CYLINDRICAL_SURFACE ( 'NONE', #1481, 5.250000000000000000 ) ;
#5336 = DIRECTION ( 'NONE',  ( 0.000000000000000000, 1.000000000000000000, 0.000000000000000000 ) ) ;
#5337 = CARTESIAN_POINT ( 'NONE',  ( 2.033577675846918216E-14, -27.81249999999999645, 5.250000000000000888 ) ) ;
#5338 = MECHANICAL_DESIGN_GEOMETRIC_PRESENTATION_REPRESENTATION (  '', ( #446 ), #3888 ) ;
#5339 = CARTESIAN_POINT ( 'NONE',  ( 5.385316468750001029, -29.22395833299193413, 3.109213912904135846 ) ) ;
#5340 = CARTESIAN_POINT ( 'NONE',  ( -4.007514324621467949, -5.149340926099361226, 1.638713065079161924 ) ) ;
#5341 = CARTESIAN_POINT ( 'NONE',  ( -1.975475456537005874E-15, -29.56250000000000000, 5.250000000000000000 ) ) ;
#5342 = CARTESIAN_POINT ( 'NONE',  ( 1.142306659890740623E-15, -28.26562499965860198, 6.218427825808274356 ) ) ;
#5343 = CARTESIAN_POINT ( 'NONE',  ( -0.01814118441313947866, -4.150659073900639484, -3.500000000000000000 ) ) ;
#5344 = EDGE_LOOP ( 'NONE', ( #8996, #7140 ) ) ;
#5345 = CARTESIAN_POINT ( 'NONE',  ( 2.625000000000000444, -28.20833333333333215, -4.546633369868303021 ) ) ;
#5346 = CIRCLE ( 'NONE', #6093, 1.500000000000000222 ) ;
#5347 = PLANE ( 'NONE',  #156 ) ;
#5348 = CARTESIAN_POINT ( 'NONE',  ( 3.616337804771879580E-16, -27.10937500034139802, -5.905927827173866440 ) ) ;
#5349 = VERTEX_POINT ( 'NONE', #5358 ) ;
#5350 = CARTESIAN_POINT ( 'NONE',  ( 5.250000000000000000, -28.87499999999999645, -6.429395695523604153E-16 ) ) ;
#5351 = AXIS2_PLACEMENT_3D ( 'NONE', #8337, #9021, #6146 ) ;
#5352 = ORIENTED_EDGE ( 'NONE', *, *, #4928, .F. ) ;
#5353 = CARTESIAN_POINT ( 'NONE',  ( 3.616337804771879580E-16, -29.04687500034139802, -5.905927827173866440 ) ) ;
#5354 = CARTESIAN_POINT ( 'NONE',  ( -2.108492589042306964, -3.249340926099361759, -2.134148098076978251 ) ) ;
#5355 = DIRECTION ( 'NONE',  ( 0.000000000000000000, -0.000000000000000000, -1.000000000000000000 ) ) ;
#5356 = CARTESIAN_POINT ( 'NONE',  ( -5.249999999999999112, -28.14583333333333215, -3.031088913245536975 ) ) ;
#5357 = CARTESIAN_POINT ( 'NONE',  ( 2.557341765625000818, -28.63020833367473017, -4.429445870380400052 ) ) ;
#5358 = CARTESIAN_POINT ( 'NONE',  ( 0.000000000000000000, 81.00000000000001421, -4.000000000000000000 ) ) ;
#5359 = CARTESIAN_POINT ( 'NONE',  ( -3.250000000000000444, 0.000000000000000000, -3.404030812060692501E-14 ) ) ;
#5360 = AXIS2_PLACEMENT_3D ( 'NONE', #3244, #447, #4725 ) ;
#5361 = CARTESIAN_POINT ( 'NONE',  ( 5.114683531249998971, -26.88020833367473017, 2.952963913586936329 ) ) ;
#5362 = ORIENTED_EDGE ( 'NONE', *, *, #191, .F. ) ;
#5363 = EDGE_CURVE ( 'NONE', #8492, #6529, #8225, .T. ) ;
#5364 = DIRECTION ( 'NONE',  ( 0.000000000000000000, 1.000000000000000000, 0.000000000000000000 ) ) ;
#5365 = CARTESIAN_POINT ( 'NONE',  ( -2.692658234375000514, -28.90104166632526983, -4.663820869356205989 ) ) ;
#5366 = CARTESIAN_POINT ( 'NONE',  ( -3.807688866302469071E-16, -29.67187499965859487, -6.218427825808274356 ) ) ;
#5367 = DIRECTION ( 'NONE',  ( 0.000000000000000000, -0.9961946980917455452, -0.08715574274765836016 ) ) ;
#5368 = CARTESIAN_POINT ( 'NONE',  ( 2.692658234374998738, -29.94270833299193413, -4.663820869356206877 ) ) ;
#5369 = CARTESIAN_POINT ( 'NONE',  ( -1.467888652719046449, -2.149340926099360782, 3.492485675378536047 ) ) ;
#5370 = ORIENTED_EDGE ( 'NONE', *, *, #173, .T. ) ;
#5371 = CARTESIAN_POINT ( 'NONE',  ( 4.898587196589411843E-16, 0.000000000000000000, 3.999999999999999112 ) ) ;
#5372 = CARTESIAN_POINT ( 'NONE',  ( 5.250000000000000000, -28.26041666734946745, -3.031088913245534755 ) ) ;
#5373 = CARTESIAN_POINT ( 'NONE',  ( 1.142306659890740623E-15, -29.29687499965860198, 6.218427825808274356 ) ) ;
#5374 = ADVANCED_FACE ( 'NONE', ( #5545 ), #4842, .T. ) ;
#5375 = ORIENTED_EDGE ( 'NONE', *, *, #1442, .F. ) ;
#5376 = CARTESIAN_POINT ( 'NONE',  ( -5.385316468750001029, -28.84895833299193413, -3.109213912904136734 ) ) ;
#5377 = CARTESIAN_POINT ( 'NONE',  ( 2.462045979635629767, -0.7506590739006389068, -2.487701488670203354 ) ) ;
#5378 = LINE ( 'NONE', #1203, #5182 ) ;
#5379 = EDGE_CURVE ( 'NONE', #4857, #6768, #1973, .T. ) ;
#5380 = DIRECTION ( 'NONE',  ( 0.000000000000000000, 0.000000000000000000, 1.000000000000000000 ) ) ;
#5381 = CARTESIAN_POINT ( 'NONE',  ( 5.249999999999999112, -27.35416666666666430, -3.031088913245536975 ) ) ;
#5382 = AXIS2_PLACEMENT_3D ( 'NONE', #7254, #2939, #4283 ) ;
#5383 = CARTESIAN_POINT ( 'NONE',  ( 5.114683531250000748, -29.35937500034139802, 0.000000000000000000 ) ) ;
#5384 = VERTEX_POINT ( 'NONE', #4111 ) ;
#5385 = SHAPE_DEFINITION_REPRESENTATION ( #5329, #4384 ) ;
#5386 = CARTESIAN_POINT ( 'NONE',  ( 1.142306659890740623E-15, -30.01562499965860198, 6.218427825808274356 ) ) ;
#5387 = CARTESIAN_POINT ( 'NONE',  ( 1.431606283892619125, -5.549340926099361582, 3.507514324621464397 ) ) ;
#5388 = CARTESIAN_POINT ( 'NONE',  ( 2.161402558328724325E-14, -29.56250000000000355, -5.250000000000000000 ) ) ;
#5389 = CARTESIAN_POINT ( 'NONE',  ( -2.692658234374996518, -28.78645833299193413, 4.663820869356208654 ) ) ;
#5390 = CARTESIAN_POINT ( 'NONE',  ( -3.507514324621434199, -7.650659073900639484, -1.431606283892695064 ) ) ;
#5391 = ORIENTED_EDGE ( 'NONE', *, *, #2072, .F. ) ;
#5392 = CARTESIAN_POINT ( 'NONE',  ( -5.249999999999997335, -30.16666666598387181, 3.031088913245538308 ) ) ;
#5393 = CARTESIAN_POINT ( 'NONE',  ( -1.000000000000000000, -35.00000000000000000, 2.880243826144208708 ) ) ;
#5394 = CARTESIAN_POINT ( 'NONE',  ( 1.431606283892694620, -4.050659073900638951, -3.507514324621433754 ) ) ;
#5395 = VECTOR ( 'NONE', #6893, 1000.000000000000000 ) ;
#5396 = CIRCLE ( 'NONE', #8820, 5.250000000000000000 ) ;
#5397 = ORIENTED_EDGE ( 'NONE', *, *, #645, .T. ) ;
#5398 = CARTESIAN_POINT ( 'NONE',  ( -5.250000000000000000, -29.02083333333333570, -3.031088913245534755 ) ) ;
#5399 = MANIFOLD_SOLID_BREP ( 'Cut-Extrude-Thin1', #6088 ) ;
#5400 = ORIENTED_EDGE ( 'NONE', *, *, #8283, .T. ) ;
#5401 = CARTESIAN_POINT ( 'NONE',  ( 2.557341765624996821, -28.90104166700806587, 4.429445870380401828 ) ) ;
#5402 = CARTESIAN_POINT ( 'NONE',  ( -3.000000000000000444, -1.849340926099361404, -0.01814118441320822922 ) ) ;
#5403 = DIRECTION ( 'NONE',  ( 0.000000000000000000, 0.000000000000000000, 1.000000000000000000 ) ) ;
#5404 = CARTESIAN_POINT ( 'NONE',  ( 2.557341765625000818, -27.13020833367473017, -4.429445870380400052 ) ) ;
#5405 = CARTESIAN_POINT ( 'NONE',  ( 0.000000000000000000, -47.00000000000000000, 0.000000000000000000 ) ) ;
#5406 = CARTESIAN_POINT ( 'NONE',  ( 0.000000000000000000, -9.000000000000000000, 2.750000000000000000 ) ) ;
#5407 = CARTESIAN_POINT ( 'NONE',  ( 2.557341765624996821, -27.15104166700806587, 4.429445870380401828 ) ) ;
#5408 = PRODUCT_RELATED_PRODUCT_CATEGORY ( 'part', '', ( #5066 ) ) ;
#5409 = CARTESIAN_POINT ( 'NONE',  ( -5.250000000000000888, -28.35416666666666785, 3.031088913245533423 ) ) ;
#5410 = CARTESIAN_POINT ( 'NONE',  ( 2.557341765624996821, -28.96354166700806587, 4.429445870380401828 ) ) ;
#5411 = DIRECTION ( 'NONE',  ( 0.000000000000000000, -1.000000000000000000, 0.000000000000000000 ) ) ;
#5412 = CARTESIAN_POINT ( 'NONE',  ( 2.692658234374998738, -28.94270833299193413, -4.663820869356206877 ) ) ;
#5413 = CARTESIAN_POINT ( 'NONE',  ( -2.692658234374996518, -30.06770833299193413, 4.663820869356208654 ) ) ;
#5414 = SURFACE_STYLE_USAGE ( .BOTH. , #2597 ) ;
#5415 = CARTESIAN_POINT ( 'NONE',  ( 5.385316468750000141, -29.23437499965859843, -6.595110575850215044E-16 ) ) ;
#5416 = CARTESIAN_POINT ( 'NONE',  ( 2.841254879263533262, -7.649340926099361226, -2.815599370228847320 ) ) ;
#5417 = ORIENTED_EDGE ( 'NONE', *, *, #8954, .T. ) ;
#5418 = CARTESIAN_POINT ( 'NONE',  ( 1.406733260263390628, -28.42633545031536713, 5.250000000000001776 ) ) ;
#5419 = CARTESIAN_POINT ( 'NONE',  ( 5.250000000000000000, -27.51041666734946389, -3.031088913245534755 ) ) ;
#5420 = CARTESIAN_POINT ( 'NONE',  ( 5.385316468750000141, -29.23437499965859843, -6.595110575850215044E-16 ) ) ;
#5421 = EDGE_LOOP ( 'NONE', ( #1985, #2491 ) ) ;
#5422 = EDGE_CURVE ( 'NONE', #5775, #6502, #7482, .T. ) ;
#5423 = CARTESIAN_POINT ( 'NONE',  ( 1.142306659890740623E-15, -28.51562499965860198, 6.218427825808274356 ) ) ;
#5424 = CARTESIAN_POINT ( 'NONE',  ( -3.500000000000000000, -2.950659073900639306, 0.01814118441314012051 ) ) ;
#5425 = DIRECTION ( 'NONE',  ( 0.000000000000000000, 0.000000000000000000, 1.000000000000000000 ) ) ;
#5426 = ADVANCED_FACE ( 'NONE', ( #6325 ), #5241, .T. ) ;
#5427 =( NAMED_UNIT ( * ) SI_UNIT ( $, .STERADIAN. ) SOLID_ANGLE_UNIT ( ) );
#5428 = LINE ( 'NONE', #3952, #8809 ) ;
#5429 = DIRECTION ( 'NONE',  ( 0.000000000000000000, -1.000000000000000000, 0.000000000000000000 ) ) ;
#5430 = EDGE_CURVE ( 'NONE', #6037, #2331, #5587, .T. ) ;
#5431 = DIRECTION ( 'NONE',  ( 0.000000000000000000, -1.000000000000000000, 0.000000000000000000 ) ) ;
#5432 = EDGE_LOOP ( 'NONE', ( #8598, #6476, #3777, #8148 ) ) ;
#5433 = SHAPE_DEFINITION_REPRESENTATION ( #4989, #6994 ) ;
#5434 = CARTESIAN_POINT ( 'NONE',  ( 2.692658234375002735, -29.74479166632526983, 4.663820869356205101 ) ) ;
#5435 = CARTESIAN_POINT ( 'NONE',  ( 3.492485675378536047, -7.349340926099362292, 1.467888652719046672 ) ) ;
#5436 = CARTESIAN_POINT ( 'NONE',  ( -2.625000000000000444, -28.04166666666666785, -4.546633369868303021 ) ) ;
#5437 = CARTESIAN_POINT ( 'NONE',  ( -5.385316468749998364, -30.05729166632526628, 3.109213912904140287 ) ) ;
#5438 = CARTESIAN_POINT ( 'NONE',  ( -3.500000000000000000, -2.950659073900639306, 0.01814118441314012051 ) ) ;
#5439 = EDGE_LOOP ( 'NONE', ( #2207, #1733, #8270, #7956 ) ) ;
#5440 = FACE_OUTER_BOUND ( 'NONE', #5781, .T. ) ;
#5441 = DIRECTION ( 'NONE',  ( 0.000000000000000000, 0.000000000000000000, -1.000000000000000000 ) ) ;
#5442 =( BOUNDED_CURVE ( )  B_SPLINE_CURVE ( 2, ( #9130, #3465, #7130, #752, #9086, #8355, #6254, #2110, #1320 ),
 .UNSPECIFIED., .F., .F. ) 
 B_SPLINE_CURVE_WITH_KNOTS ( ( 3, 2, 2, 2, 3 ),
 ( 0.06250000000000000000, 0.06944444444444444753, 0.08333333333333332871, 0.09722222222222222376, 0.1041666666666666713 ),
 .UNSPECIFIED. ) 
 CURVE ( )  GEOMETRIC_REPRESENTATION_ITEM ( )  RATIONAL_B_SPLINE_CURVE ( ( 0.9330127018922194093, 0.9330127018922194093, 1.000000000000000000, 0.8660254037844387076, 1.000000000000000000, 0.8660254037844387076, 1.000000000000000000, 0.9330127018922192983, 0.9330127018922194093 ) ) 
 REPRESENTATION_ITEM ( '' )  );
#5443 = CARTESIAN_POINT ( 'NONE',  ( 1.431606283892694620, -2.450659073900638862, -3.507514324621433754 ) ) ;
#5444 = ORIENTED_EDGE ( 'NONE', *, *, #5041, .T. ) ;
#5445 = FILL_AREA_STYLE ('',( #3968 ) ) ;
#5446 = CARTESIAN_POINT ( 'NONE',  ( -2.625000000000000444, -28.79166666666666785, -4.546633369868303021 ) ) ;
#5447 = ORIENTED_EDGE ( 'NONE', *, *, #8719, .T. ) ;
#5448 = APPLICATION_CONTEXT ( 'automotive_design' ) ;
#5449 = CARTESIAN_POINT ( 'NONE',  ( -2.557341765624999042, -28.77604166700806587, -4.429445870380400052 ) ) ;
#5450 = CARTESIAN_POINT ( 'NONE',  ( -0.01814118441320841310, -2.249340926099360871, 3.000000000000000444 ) ) ;
#5451 = CARTESIAN_POINT ( 'NONE',  ( -9.180150650966086169E-15, -28.18749999999999645, 5.249999999999999112 ) ) ;
#5452 = CARTESIAN_POINT ( 'NONE',  ( 3.616337804771879580E-16, -27.10937500034139802, -5.905927827173866440 ) ) ;
#5453 = CARTESIAN_POINT ( 'NONE',  ( -1.406733260263402174, -29.13616454900182973, 5.249999999999995559 ) ) ;
#5454 = EDGE_CURVE ( 'NONE', #6825, #1943, #1988, .T. ) ;
#5455 = CARTESIAN_POINT ( 'NONE',  ( -5.114683531249999859, -27.00520833367473017, -2.952963913586935440 ) ) ;
#5456 = CARTESIAN_POINT ( 'NONE',  ( 0.000000000000000000, -20.00000000000000000, 0.000000000000000000 ) ) ;
#5457 = CARTESIAN_POINT ( 'NONE',  ( 3.616337804771879580E-16, -28.60937500034139802, -5.905927827173866440 ) ) ;
#5458 = MECHANICAL_DESIGN_GEOMETRIC_PRESENTATION_REPRESENTATION (  '', ( #4272 ), #2053 ) ;
#5459 = FACE_OUTER_BOUND ( 'NONE', #2206, .T. ) ;
#5460 = CARTESIAN_POINT ( 'NONE',  ( -2.692658234374996518, -29.06770833299193413, 4.663820869356208654 ) ) ;
#5461 = CARTESIAN_POINT ( 'NONE',  ( -1.406733260263393293, -28.67633545031537068, -5.250000000000000000 ) ) ;
#5462 = CARTESIAN_POINT ( 'NONE',  ( -5.385316468749998364, -29.83854166632526628, 3.109213912904140287 ) ) ;
#5463 = CARTESIAN_POINT ( 'NONE',  ( 3.507514324621465285, -5.949340926099361937, -1.431606283892619125 ) ) ;
#5464 = CARTESIAN_POINT ( 'NONE',  ( -3.992485675378532939, -6.549340926099361582, -1.674995433905601683 ) ) ;
#5465 = ORIENTED_EDGE ( 'NONE', *, *, #4971, .F. ) ;
#5466 = CARTESIAN_POINT ( 'NONE',  ( 0.000000000000000000, -35.00000000000000000, 0.000000000000000000 ) ) ;
#5467 = CARTESIAN_POINT ( 'NONE',  ( -5.250000000000000888, -27.63541666734946034, 3.031088913245532979 ) ) ;
#5468 =( GEOMETRIC_REPRESENTATION_CONTEXT ( 3 ) GLOBAL_UNCERTAINTY_ASSIGNED_CONTEXT ( ( #1804 ) ) GLOBAL_UNIT_ASSIGNED_CONTEXT ( ( #654, #7861, #6319 ) ) REPRESENTATION_CONTEXT ( 'NONE', 'WORKASPACE' ) );
#5469 = CARTESIAN_POINT ( 'NONE',  ( -2.692658234375000514, -29.90104166632526983, -4.663820869356205989 ) ) ;
#5470 = ORIENTED_EDGE ( 'NONE', *, *, #8443, .T. ) ;
#5471 = CARTESIAN_POINT ( 'NONE',  ( -2.692658234375000514, -28.61979166632526628, -4.663820869356205989 ) ) ;
#5472 = CARTESIAN_POINT ( 'NONE',  ( -2.462045979635629323, 0.04934092609936105434, 2.487701488670203798 ) ) ;
#5473 = CARTESIAN_POINT ( 'NONE',  ( 6.972266317189433020E-16, -29.71875000068279249, -5.250000000000000000 ) ) ;
#5474 = LINE ( 'NONE', #4223, #8493 ) ;
#5475 = DIRECTION ( 'NONE',  ( 0.000000000000000000, 1.000000000000000000, 0.000000000000000000 ) ) ;
#5476 = DIRECTION ( 'NONE',  ( 0.000000000000000000, 0.000000000000000000, 1.000000000000000000 ) ) ;
#5477 = CIRCLE ( 'NONE', #1462, 0.2499999999999998335 ) ;
#5478 = CARTESIAN_POINT ( 'NONE',  ( 5.114683531249999859, -29.83854166700806587, -2.952963913586932776 ) ) ;
#5479 = CARTESIAN_POINT ( 'NONE',  ( 6.429395695523604153E-16, 75.00000000000000000, -5.250000000000000000 ) ) ;
#5480 =( NAMED_UNIT ( * ) SI_UNIT ( $, .STERADIAN. ) SOLID_ANGLE_UNIT ( ) );
#5481 = CARTESIAN_POINT ( 'NONE',  ( -2.692658234374996518, -29.53645833299193413, 4.663820869356208654 ) ) ;
#5482 = CARTESIAN_POINT ( 'NONE',  ( 0.01814118441321408565, -7.849340926099360516, -3.500000000000000000 ) ) ;
#5483 = ADVANCED_FACE ( 'NONE', ( #6286 ), #53, .F. ) ;
#5484 = CARTESIAN_POINT ( 'NONE',  ( 5.249999999999999112, -28.54166666598386470, -3.031088913245536975 ) ) ;
#5485 = CARTESIAN_POINT ( 'NONE',  ( 2.692658234374998738, -29.91145833299193413, -4.663820869356206877 ) ) ;
#5486 = CARTESIAN_POINT ( 'NONE',  ( 1.467888652718972731, -3.450659073900638862, 3.492485675378566246 ) ) ;
#5487 = CARTESIAN_POINT ( 'NONE',  ( -5.249999999999999112, -27.17708333401612819, -3.031088913245536975 ) ) ;
#5488 = VECTOR ( 'NONE', #8452, 1000.000000000000000 ) ;
#5489 = FACE_BOUND ( 'NONE', #4060, .T. ) ;
#5490 = CARTESIAN_POINT ( 'NONE',  ( -3.492485675378566246, -4.650659073900639484, 1.467888652718973175 ) ) ;
#5491 = EDGE_LOOP ( 'NONE', ( #5301, #2230, #6170, #353 ) ) ;
#5492 =( NAMED_UNIT ( * ) SI_UNIT ( $, .STERADIAN. ) SOLID_ANGLE_UNIT ( ) );
#5493 = VECTOR ( 'NONE', #3986, 1000.000000000000000 ) ;
#5494 = CLOSED_SHELL ( 'NONE', ( #1290, #1805, #6438, #578, #2561, #2134 ) ) ;
#5495 = CARTESIAN_POINT ( 'NONE',  ( 5.250000000000000000, -27.87500000000000000, -6.429395695523604153E-16 ) ) ;
#5496 = ADVANCED_FACE ( 'NONE', ( #2190 ), #4153, .F. ) ;
#5497 = CARTESIAN_POINT ( 'NONE',  ( 5.114683531250000748, -27.58854166700806587, -2.952963913586932776 ) ) ;
#5498 = CARTESIAN_POINT ( 'NONE',  ( 1.260781871532495657, -1.349340926099361626, -2.992485675378538268 ) ) ;
#5499 = CARTESIAN_POINT ( 'NONE',  ( 1.406733260263398400, -28.07366454968463287, -5.249999999999997335 ) ) ;
#5500 = CIRCLE ( 'NONE', #7734, 6.250000000000000000 ) ;
#5501 = CARTESIAN_POINT ( 'NONE',  ( 5.250000000000000000, -29.97916666666666430, -3.031088913245534755 ) ) ;
#5502 = DIRECTION ( 'NONE',  ( 1.000000000000000000, 0.000000000000000000, 0.000000000000000000 ) ) ;
#5503 = B_SPLINE_CURVE_WITH_KNOTS ( 'NONE', 3,
 ( #5359, #4191, #8423, #7554, #7023, #650, #1180, #4024, #1090, #1791, #6011, #3932, #6859, #5311, #8849, #2052, #5967, #3327 ),
 .UNSPECIFIED., .F., .F.,
 ( 4, 2, 2, 2, 2, 2, 2, 2, 4 ),
 ( 0.000000000000000000, 0.001653989080654771947, 0.002480983620982158029, 0.002894480891145850745, 0.003101229526227697320, 0.003204603843768620824, 0.003256291002539082359, 0.003282134581924312476, 0.003307978161309543027 ),
 .UNSPECIFIED. ) ;
#5504 =( BOUNDED_CURVE ( )  B_SPLINE_CURVE ( 2, ( #4869, #7810, #5614, #1344, #4268, #8462, #775, #3575, #5748 ),
 .UNSPECIFIED., .F., .F. ) 
 B_SPLINE_CURVE_WITH_KNOTS ( ( 3, 2, 2, 2, 3 ),
 ( 0.2291666666666666574, 0.2361111111111111049, 0.2500000000000000000, 0.2638888888888888951, 0.2708333333333333148 ),
 .UNSPECIFIED. ) 
 CURVE ( )  GEOMETRIC_REPRESENTATION_ITEM ( )  RATIONAL_B_SPLINE_CURVE ( ( 0.9330127018922194093, 0.9330127018922194093, 1.000000000000000000, 0.8660254037844387076, 1.000000000000000000, 0.8660254037844387076, 1.000000000000000000, 0.9330127018922196314, 0.9330127018922194093 ) ) 
 REPRESENTATION_ITEM ( '' )  );
#5505 = CARTESIAN_POINT ( 'NONE',  ( 2.557341765625000818, -28.88020833367473017, -4.429445870380400052 ) ) ;
#5506 = CIRCLE ( 'NONE', #6100, 3.000000000000000444 ) ;
#5507 = FACE_OUTER_BOUND ( 'NONE', #1830, .T. ) ;
#5508 = CARTESIAN_POINT ( 'NONE',  ( -5.114683531250000748, -28.79687500034139802, -6.263680815196995234E-16 ) ) ;
#5509 = CYLINDRICAL_SURFACE ( 'NONE', #7858, 5.250000000000000000 ) ;
#5510 = CARTESIAN_POINT ( 'NONE',  ( -5.250000000000000000, -28.70833333265053611, -3.031088913245534755 ) ) ;
#5511 = CARTESIAN_POINT ( 'NONE',  ( -2.624999999999998668, -29.19791666734946389, -4.546633369868303021 ) ) ;
#5512 =( LENGTH_UNIT ( ) NAMED_UNIT ( * ) SI_UNIT ( .MILLI., .METRE. ) );
#5513 = CARTESIAN_POINT ( 'NONE',  ( 5.385316468750001029, -29.75520833299193413, 3.109213912904135846 ) ) ;
#5514 = CARTESIAN_POINT ( 'NONE',  ( -3.507514324621464397, -1.949340926099361271, 1.431606283892619347 ) ) ;
#5515 = CARTESIAN_POINT ( 'NONE',  ( 4.007514324621469726, -5.949340926099362825, -1.638713065079161257 ) ) ;
#5516 = ORIENTED_EDGE ( 'NONE', *, *, #6725, .F. ) ;
#5517 = CARTESIAN_POINT ( 'NONE',  ( 2.033577675846918216E-14, -27.81249999999999645, 5.250000000000000888 ) ) ;
#5518 = CARTESIAN_POINT ( 'NONE',  ( 3.712013335537174572E-16, -28.46875000068279249, -6.062177826491070398 ) ) ;
#5519 = CARTESIAN_POINT ( 'NONE',  ( 5.385316468750001029, -29.50520833299193413, 3.109213912904135846 ) ) ;
#5520 = ORIENTED_EDGE ( 'NONE', *, *, #4023, .F. ) ;
#5521 = CARTESIAN_POINT ( 'NONE',  ( -2.692658234374996518, -29.53645833299193413, 4.663820869356208654 ) ) ;
#5522 = CARTESIAN_POINT ( 'NONE',  ( -1.260781871532431708, -7.450659073900640195, -2.992485675378564469 ) ) ;
#5523 = CYLINDRICAL_SURFACE ( 'NONE', #9186, 5.250000000000000000 ) ;
#5524 =( BOUNDED_CURVE ( )  B_SPLINE_CURVE ( 2, ( #1412, #7968, #8664, #7833, #3002, #1499, #5684, #7132, #4252 ),
 .UNSPECIFIED., .F., .T. ) 
 B_SPLINE_CURVE_WITH_KNOTS ( ( 3, 2, 2, 2, 3 ),
 ( 0.02083333333333333218, 0.02777777777777777624, 0.04166666666666666435, 0.05555555555555555247, 0.06250000000000000000 ),
 .UNSPECIFIED. ) 
 CURVE ( )  GEOMETRIC_REPRESENTATION_ITEM ( )  RATIONAL_B_SPLINE_CURVE ( ( 0.9330127018922194093, 0.9330127018922194093, 1.000000000000000000, 0.8660254037844387076, 1.000000000000000000, 0.8660254037844387076, 1.000000000000000000, 0.9330127018922194093, 0.9330127018922194093 ) ) 
 REPRESENTATION_ITEM ( '' )  );
#5525 = ADVANCED_FACE ( 'NONE', ( #8562 ), #4334, .T. ) ;
#5526 = PRESENTATION_STYLE_ASSIGNMENT (( #7526 ) ) ;
#5527 = DIRECTION ( 'NONE',  ( 0.000000000000000000, -1.000000000000000000, 0.000000000000000000 ) ) ;
#5528 = CARTESIAN_POINT ( 'NONE',  ( 0.01814118441321408565, -7.849340926099360516, -3.500000000000000000 ) ) ;
#5529 = CARTESIAN_POINT ( 'NONE',  ( -5.114683531250000748, -28.23437500034139447, -6.263680815196995234E-16 ) ) ;
#5530 = DIRECTION ( 'NONE',  ( 0.000000000000000000, -1.000000000000000000, 0.000000000000000000 ) ) ;
#5531 = APPLICATION_CONTEXT ( 'automotive_design' ) ;
#5532 = CARTESIAN_POINT ( 'NONE',  ( 2.692658234374998738, -29.66145833299193413, -4.663820869356206877 ) ) ;
#5533 = CARTESIAN_POINT ( 'NONE',  ( -2.487701488670255312, -6.849340926099361404, 2.462045979635577808 ) ) ;
#5534 = CARTESIAN_POINT ( 'NONE',  ( -3.500000000000000000, -0.2493409260993610654, -0.01814118441321343686 ) ) ;
#5535 = CARTESIAN_POINT ( 'NONE',  ( 2.692658234375002735, -29.99479166632526628, 4.663820869356205101 ) ) ;
#5536 = CARTESIAN_POINT ( 'NONE',  ( 1.674995433905515085, -5.050659073900638951, 3.992485675378568022 ) ) ;
#5537 = CARTESIAN_POINT ( 'NONE',  ( 2.624999999999998668, -30.02083333265053611, -4.546633369868303021 ) ) ;
#5538 = CYLINDRICAL_SURFACE ( 'NONE', #1351, 5.250000000000000000 ) ;
#5539 = ORIENTED_EDGE ( 'NONE', *, *, #7576, .T. ) ;
#5540 = CARTESIAN_POINT ( 'NONE',  ( -2.625000000000000444, -28.04166666666666785, -4.546633369868303021 ) ) ;
#5541 = AXIS2_PLACEMENT_3D ( 'NONE', #2027, #6255, #7042 ) ;
#5542 = CARTESIAN_POINT ( 'NONE',  ( -5.114683531250000748, -27.73437500034139802, -6.263680815196995234E-16 ) ) ;
#5543 = CARTESIAN_POINT ( 'NONE',  ( -2.992485675378538268, -8.149340926099366555, -1.260781871532495879 ) ) ;
#5544 = CARTESIAN_POINT ( 'NONE',  ( -5.114683531250000748, -27.29687500034139802, -6.263680815196995234E-16 ) ) ;
#5545 = FACE_OUTER_BOUND ( 'NONE', #585, .T. ) ;
#5546 = AXIS2_PLACEMENT_3D ( 'NONE', #7287, #1472, #6443 ) ;
#5547 = CARTESIAN_POINT ( 'NONE',  ( -1.084901341431563726E-15, -29.48437500034139802, 5.905927827173866440 ) ) ;
#5548 = EDGE_CURVE ( 'NONE', #4820, #4350, #793, .T. ) ;
#5549 = CARTESIAN_POINT ( 'NONE',  ( 2.557341765625000818, -29.63020833367473017, -4.429445870380400052 ) ) ;
#5550 = FACE_OUTER_BOUND ( 'NONE', #8624, .T. ) ;
#5551 = CARTESIAN_POINT ( 'NONE',  ( -5.250000000000000000, -29.43749999931720041, 0.000000000000000000 ) ) ;
#5552 = DIRECTION ( 'NONE',  ( 0.000000000000000000, 0.000000000000000000, -1.000000000000000000 ) ) ;
#5553 = AXIS2_PLACEMENT_3D ( 'NONE', #1957, #6929, #6183 ) ;
#5554 = CARTESIAN_POINT ( 'NONE',  ( -1.925759277493323207, -9.035843541029837430E-14, 2.922632427747480222 ) ) ;
#5555 = CARTESIAN_POINT ( 'NONE',  ( 5.250000000000000000, -28.49999999999999645, 0.000000000000000000 ) ) ;
#5556 = CARTESIAN_POINT ( 'NONE',  ( -1.467888652719046449, -3.749340926099360871, 3.492485675378536047 ) ) ;
#5557 = CARTESIAN_POINT ( 'NONE',  ( 4.007514324621469726, -7.549340926099361582, -1.638713065079161257 ) ) ;
#5558 = ORIENTED_EDGE ( 'NONE', *, *, #1888, .T. ) ;
#5559 = CARTESIAN_POINT ( 'NONE',  ( -2.625000000000000444, -27.54166666666666430, -4.546633369868303021 ) ) ;
#5560 = CARTESIAN_POINT ( 'NONE',  ( 2.625000000000000444, -27.23958333401612819, -4.546633369868303021 ) ) ;
#5561 = CARTESIAN_POINT ( 'NONE',  ( -2.692658234374996518, -30.06770833299193413, 4.663820869356208654 ) ) ;
#5562 = EDGE_LOOP ( 'NONE', ( #2669, #6524, #8541, #4708 ) ) ;
#5563 = CARTESIAN_POINT ( 'NONE',  ( 2.692658234375002735, -29.74479166632526983, 4.663820869356205101 ) ) ;
#5564 = CARTESIAN_POINT ( 'NONE',  ( -3.500000000000000000, -6.150659073900639484, 0.01814118441314012051 ) ) ;
#5565 = CARTESIAN_POINT ( 'NONE',  ( -5.250000000000000888, -27.10416666666666430, 3.031088913245533423 ) ) ;
#5566 = DIRECTION ( 'NONE',  ( -0.8660254037844402619, -0.4999999999999970579, 0.000000000000000000 ) ) ;
#5567 = DIRECTION ( 'NONE',  ( -0.000000000000000000, 1.000000000000000000, -0.000000000000000000 ) ) ;
#5568 = EDGE_CURVE ( 'NONE', #4568, #296, #3502, .T. ) ;
#5569 = CARTESIAN_POINT ( 'NONE',  ( 2.487701488670255756, -6.049340926099361582, -2.462045979635577364 ) ) ;
#5570 = CARTESIAN_POINT ( 'NONE',  ( 5.114683531250000748, -28.85937500034139802, 0.000000000000000000 ) ) ;
#5571 = CARTESIAN_POINT ( 'NONE',  ( -1.406733260263389518, -28.23883544963256753, -5.250000000000001776 ) ) ;
#5572 = CARTESIAN_POINT ( 'NONE',  ( -1.975475456537005874E-15, -29.09375000068279249, 5.249999999999999112 ) ) ;
#5573 = CARTESIAN_POINT ( 'NONE',  ( 3.500000000000000000, -7.449340926099361937, 0.01814118441321387054 ) ) ;
#5574 = CARTESIAN_POINT ( 'NONE',  ( 0.000000000000000000, -9.999999999999998224, 0.000000000000000000 ) ) ;
#5575 =( BOUNDED_CURVE ( )  B_SPLINE_CURVE ( 2, ( #6833, #9101, #3254, #5381, #3999, #1206, #8233, #1155, #458 ),
 .UNSPECIFIED., .F., .T. ) 
 B_SPLINE_CURVE_WITH_KNOTS ( ( 3, 2, 2, 2, 3 ),
 ( 0.1041666666666666713, 0.1111111111111111049, 0.1250000000000000000, 0.1388888888888888951, 0.1458333333333333426 ),
 .UNSPECIFIED. ) 
 CURVE ( )  GEOMETRIC_REPRESENTATION_ITEM ( )  RATIONAL_B_SPLINE_CURVE ( ( 0.9330127018922194093, 0.9330127018922194093, 1.000000000000000000, 0.8660254037844387076, 1.000000000000000000, 0.8660254037844387076, 1.000000000000000000, 0.9330127018922194093, 0.9330127018922194093 ) ) 
 REPRESENTATION_ITEM ( '' )  );
#5576 = CARTESIAN_POINT ( 'NONE',  ( 5.385316468749999252, -29.93229166632526983, -3.109213912904139399 ) ) ;
#5577 = CARTESIAN_POINT ( 'NONE',  ( 2.815599370228907716, -3.950659073900640195, -2.841254879263473310 ) ) ;
#5578 = CARTESIAN_POINT ( 'NONE',  ( 6.972266317189433020E-16, -27.71875000068279604, -5.249999999999999112 ) ) ;
#5579 = PRODUCT_RELATED_PRODUCT_CATEGORY ( 'part', '', ( #4921 ) ) ;
#5580 = FILL_AREA_STYLE_COLOUR ( '', #6851 ) ;
#5581 = DIRECTION ( 'NONE',  ( 0.000000000000000000, 0.000000000000000000, -1.000000000000000000 ) ) ;
#5582 = ORIENTED_EDGE ( 'NONE', *, *, #7243, .F. ) ;
#5583 = CARTESIAN_POINT ( 'NONE',  ( -5.385316468750001029, -27.09895833299193413, -3.109213912904136734 ) ) ;
#5584 = CARTESIAN_POINT ( 'NONE',  ( -2.557341765624999042, -28.02604166700806587, -4.429445870380400052 ) ) ;
#5585 = CARTESIAN_POINT ( 'NONE',  ( -1.260781871532431708, -2.650659073900639928, -2.992485675378564469 ) ) ;
#5586 = CARTESIAN_POINT ( 'NONE',  ( -1.084901341431563923E-15, -27.48437500034140157, 5.905927827173866440 ) ) ;
#5587 = LINE ( 'NONE', #2104, #8656 ) ;
#5588 = EDGE_CURVE ( 'NONE', #4395, #3470, #1996, .T. ) ;
#5589 = CARTESIAN_POINT ( 'NONE',  ( 2.557341765625000818, -29.63020833367473017, -4.429445870380400052 ) ) ;
#5590 = LINE ( 'NONE', #7739, #2535 ) ;
#5591 = CARTESIAN_POINT ( 'NONE',  ( -2.557341765625002594, -29.00520833367473017, 4.429445870380399164 ) ) ;
#5592 = DIRECTION ( 'NONE',  ( 0.000000000000000000, -1.000000000000000000, 0.000000000000000000 ) ) ;
#5593 = CARTESIAN_POINT ( 'NONE',  ( 1.113604000661152470E-15, -29.37499999931719685, 6.062177826491070398 ) ) ;
#5594 = CARTESIAN_POINT ( 'NONE',  ( 1.406733260263394847, -27.51116454900183683, -5.250000000000000000 ) ) ;
#5595 = ADVANCED_FACE ( 'NONE', ( #5012 ), #93, .T. ) ;
#5596 = CARTESIAN_POINT ( 'NONE',  ( -1.406733260263393959, -27.23883544963257108, -5.250000000000000888 ) ) ;
#5597 = CARTESIAN_POINT ( 'NONE',  ( -1.431606283892620235, -1.549340926099361138, -3.507514324621463953 ) ) ;
#5598 = CARTESIAN_POINT ( 'NONE',  ( 2.462045979635577364, -4.049340926099360694, 2.487701488670255312 ) ) ;
#5599 = EDGE_LOOP ( 'NONE', ( #2188, #8815 ) ) ;
#5600 = CARTESIAN_POINT ( 'NONE',  ( 2.625000000000002220, -29.16666666666666785, 4.546633369868302132 ) ) ;
#5601 = CARTESIAN_POINT ( 'NONE',  ( -2.624999999999998668, -26.94791666734946389, -4.546633369868303021 ) ) ;
#5602 = MECHANICAL_DESIGN_GEOMETRIC_PRESENTATION_REPRESENTATION (  '', ( #2340 ), #4717 ) ;
#5603 = ORIENTED_EDGE ( 'NONE', *, *, #3267, .T. ) ;
#5604 = CARTESIAN_POINT ( 'NONE',  ( -5.385316468750001029, -29.09895833299193058, -3.109213912904136734 ) ) ;
#5605 = CARTESIAN_POINT ( 'NONE',  ( -4.007514324621431534, -1.250659073900638685, -1.638713065079248521 ) ) ;
#5606 = CARTESIAN_POINT ( 'NONE',  ( -5.250000000000000000, -27.12500000000000000, -6.429395695523604153E-16 ) ) ;
#5607 = ORIENTED_EDGE ( 'NONE', *, *, #6672, .F. ) ;
#5608 = COLOUR_RGB ( '',0.8941176470588234615, 0.8941176470588234615, 0.8941176470588234615 ) ;
#5609 = DIRECTION ( 'NONE',  ( 0.000000000000000000, -1.000000000000000000, 0.000000000000000000 ) ) ;
#5610 = FACE_OUTER_BOUND ( 'NONE', #4906, .T. ) ;
#5611 = FACE_OUTER_BOUND ( 'NONE', #388, .T. ) ;
#5612 = CARTESIAN_POINT ( 'NONE',  ( 3.616337804771879580E-16, -28.54687500034139802, -5.905927827173866440 ) ) ;
#5613 = CARTESIAN_POINT ( 'NONE',  ( 4.898587196589411843E-16, 1.000000000000000000, 3.999999999999999112 ) ) ;
#5614 = CARTESIAN_POINT ( 'NONE',  ( 2.624999999999996891, -29.07291666734946389, 4.546633369868304797 ) ) ;
#5615 = CARTESIAN_POINT ( 'NONE',  ( 0.01814118441320878086, -1.449340926099361493, -3.000000000000000444 ) ) ;
#5616 = CARTESIAN_POINT ( 'NONE',  ( 1.045839947578414884E-14, -28.24999999931720041, -5.249999999999999112 ) ) ;
#5617 = CARTESIAN_POINT ( 'NONE',  ( 5.385316468749999252, -27.21354166632526628, -3.109213912904139399 ) ) ;
#5618 = ADVANCED_FACE ( 'NONE', ( #4243, #3590 ), #2901, .F. ) ;
#5619 = CARTESIAN_POINT ( 'NONE',  ( 4.007514324621432422, -0.4506590739006384738, 1.638713065079246078 ) ) ;
#5620 = FACE_BOUND ( 'NONE', #5324, .T. ) ;
#5621 = CARTESIAN_POINT ( 'NONE',  ( 0.000000000000000000, -20.00000000000000000, -2.000000000000000000 ) ) ;
#5622 = ORIENTED_EDGE ( 'NONE', *, *, #1249, .T. ) ;
#5623 =( BOUNDED_CURVE ( )  B_SPLINE_CURVE ( 2, ( #965, #8783, #4599, #2462, #1572, #3769, #4414, #1619, #8735 ),
 .UNSPECIFIED., .F., .T. ) 
 B_SPLINE_CURVE_WITH_KNOTS ( ( 3, 2, 2, 2, 3 ),
 ( 0.1458333333333333426, 0.1527777777777777901, 0.1666666666666666574, 0.1805555555555555525, 0.1875000000000000000 ),
 .UNSPECIFIED. ) 
 CURVE ( )  GEOMETRIC_REPRESENTATION_ITEM ( )  RATIONAL_B_SPLINE_CURVE ( ( 0.9330127018922194093, 0.9330127018922194093, 1.000000000000000000, 0.8660254037844387076, 1.000000000000000000, 0.8660254037844387076, 1.000000000000000000, 0.9330127018922194093, 0.9330127018922194093 ) ) 
 REPRESENTATION_ITEM ( '' )  );
#5624 = CARTESIAN_POINT ( 'NONE',  ( -5.250000000000000000, -29.77083333333333570, -3.031088913245534755 ) ) ;
#5625 = CIRCLE ( 'NONE', #6826, 5.250000000000000000 ) ;
#5626 = EDGE_CURVE ( 'NONE', #7281, #7319, #8591, .T. ) ;
#5627 = CARTESIAN_POINT ( 'NONE',  ( 3.616337804771879580E-16, -27.54687500034139802, -5.905927827173866440 ) ) ;
#5628 = CARTESIAN_POINT ( 'NONE',  ( -2.108492589042352261, 0.04934092609936062412, 2.134148098076933397 ) ) ;
#5629 = CARTESIAN_POINT ( 'NONE',  ( -1.113604000661152470E-15, -28.81249999999999645, 6.062177826491070398 ) ) ;
#5630 = DIRECTION ( 'NONE',  ( 0.000000000000000000, 0.000000000000000000, -1.000000000000000000 ) ) ;
#5631 = CARTESIAN_POINT ( 'NONE',  ( -5.114683531250000748, -29.79687500034139802, -6.263680815196995234E-16 ) ) ;
#5632=STYLED_ITEM('',(#9218),#8468);
#5633 = SHAPE_REPRESENTATION_RELATIONSHIP ( 'NONE' , 'NONE' ,  #3200, #417 ) ;
#5634 = CARTESIAN_POINT ( 'NONE',  ( -2.557341765625002594, -27.25520833367473017, 4.429445870380399164 ) ) ;
#5635 = CONICAL_SURFACE ( 'NONE', #1057, 2.750000000000000000, 0.08726646259971666819 ) ;
#5636 = CARTESIAN_POINT ( 'NONE',  ( -1.406733260263384411, -29.30133545031537068, -5.250000000000006217 ) ) ;
#5637 = CARTESIAN_POINT ( 'NONE',  ( -2.624999999999996891, -29.14583333265053611, 4.546633369868304797 ) ) ;
#5638 = FACE_OUTER_BOUND ( 'NONE', #5010, .T. ) ;
#5639 = CARTESIAN_POINT ( 'NONE',  ( 0.000000000000000000, -20.00000000000000000, 0.000000000000000000 ) ) ;
#5640 = CARTESIAN_POINT ( 'NONE',  ( 2.462045979635577364, -5.649340926099361226, 2.487701488670255312 ) ) ;
#5641 = CIRCLE ( 'NONE', #1338, 2.629341307491595447 ) ;
#5642 = PRESENTATION_STYLE_ASSIGNMENT (( #1452 ) ) ;
#5643 = VERTEX_POINT ( 'NONE', #5062 ) ;
#5644 = CARTESIAN_POINT ( 'NONE',  ( -2.625000000000000444, -29.72916666598387181, -4.546633369868303021 ) ) ;
#5645 = CIRCLE ( 'NONE', #4169, 2.499999999999999556 ) ;
#5646 = CARTESIAN_POINT ( 'NONE',  ( -2.557341765625002594, -29.19270833367473017, 4.429445870380399164 ) ) ;
#5647 = EDGE_CURVE ( 'NONE', #7496, #8472, #1693, .T. ) ;
#5648 = ORIENTED_EDGE ( 'NONE', *, *, #3349, .F. ) ;
#5649 = CARTESIAN_POINT ( 'NONE',  ( 2.692658234375002735, -29.49479166632526983, 4.663820869356205101 ) ) ;
#5650 = CARTESIAN_POINT ( 'NONE',  ( 3.507514324621434199, -6.850659073900638774, 1.431606283892693066 ) ) ;
#5651 = LINE ( 'NONE', #6266, #6509 ) ;
#5652 = ORIENTED_EDGE ( 'NONE', *, *, #7383, .T. ) ;
#5653 = LINE ( 'NONE', #678, #4911 ) ;
#5654 = LINE ( 'NONE', #1423, #6148 ) ;
#5655 = EDGE_CURVE ( 'NONE', #4378, #1880, #5789, .T. ) ;
#5656 = CARTESIAN_POINT ( 'NONE',  ( 6.972266317189434006E-16, -27.24999999931720751, -5.250000000000000000 ) ) ;
#5657 = VECTOR ( 'NONE', #3847, 1000.000000000000000 ) ;
#5658 = CARTESIAN_POINT ( 'NONE',  ( 5.114683531250000748, -29.10937500034139802, 0.000000000000000000 ) ) ;
#5659 = CARTESIAN_POINT ( 'NONE',  ( 7.654042494670957606E-16, 69.99999999999998579, -6.250000000000000000 ) ) ;
#5660 = CARTESIAN_POINT ( 'NONE',  ( 0.000000000000000000, -46.00000000000000000, 0.000000000000000000 ) ) ;
#5661 = EDGE_CURVE ( 'NONE', #5696, #7888, #6781, .T. ) ;
#5662 = CARTESIAN_POINT ( 'NONE',  ( 1.224499502706077214, -3.949340926099361493, 3.007514324621463508 ) ) ;
#5663 = CARTESIAN_POINT ( 'NONE',  ( 2.161402558328724325E-14, -28.56250000000000000, -5.250000000000000000 ) ) ;
#5664 = CARTESIAN_POINT ( 'NONE',  ( -2.692658234374996518, -27.81770833299193413, 4.663820869356208654 ) ) ;
#5665 = CARTESIAN_POINT ( 'NONE',  ( 0.01814118441313467001, -4.950659073900639306, 4.000000000000000000 ) ) ;
#5666 = FACE_BOUND ( 'NONE', #8123, .T. ) ;
#5667 = CARTESIAN_POINT ( 'NONE',  ( -5.249999999999999112, -27.89583333333332860, -3.031088913245536975 ) ) ;
#5668 = ORIENTED_EDGE ( 'NONE', *, *, #698, .F. ) ;
#5669 = SHAPE_REPRESENTATION_RELATIONSHIP ( 'NONE' , 'NONE' ,  #2490, #6298 ) ;
#5670 = CARTESIAN_POINT ( 'NONE',  ( -5.249999999999999112, -29.22916666666666430, 3.031088913245538308 ) ) ;
#5671 = CARTESIAN_POINT ( 'NONE',  ( -2.557341765624999042, -27.77604166700806587, -4.429445870380400052 ) ) ;
#5672 = CARTESIAN_POINT ( 'NONE',  ( 0.01814118441314514080, -1.750659073900639351, 3.000000000000000444 ) ) ;
#5673 = CARTESIAN_POINT ( 'NONE',  ( -5.250000000000000000, -28.89583333333333215, -3.031088913245536531 ) ) ;
#5674 =( NAMED_UNIT ( * ) PLANE_ANGLE_UNIT ( ) SI_UNIT ( $, .RADIAN. ) );
#5675 = CARTESIAN_POINT ( 'NONE',  ( -2.557341765625002594, -29.50520833367473017, 4.429445870380399164 ) ) ;
#5676 = AXIS2_PLACEMENT_3D ( 'NONE', #5246, #1718, #6685 ) ;
#5677 = VECTOR ( 'NONE', #3426, 1000.000000000000000 ) ;
#5678 = CARTESIAN_POINT ( 'NONE',  ( -5.114683531249999859, -27.31770833367473017, -2.952963913586935440 ) ) ;
#5679 = CARTESIAN_POINT ( 'NONE',  ( -5.250000000000000000, -28.95833333265053255, -3.031088913245534755 ) ) ;
#5680 = CARTESIAN_POINT ( 'NONE',  ( -1.000000000000000000, -29.00000000000000355, -2.431755684948965435 ) ) ;
#5681 = CARTESIAN_POINT ( 'NONE',  ( -2.281106635417135653, -1.535234168922110014E-16, 2.799845732222085992 ) ) ;
#5682 = VECTOR ( 'NONE', #3028, 1000.000000000000000 ) ;
#5683 = CYLINDRICAL_SURFACE ( 'NONE', #7768, 3.000000000000000444 ) ;
#5684 = CARTESIAN_POINT ( 'NONE',  ( -2.625000000000002220, -29.61458333401613174, 4.546633369868302132 ) ) ;
#5685 = CARTESIAN_POINT ( 'NONE',  ( -2.487701488670255312, -5.249340926099360871, 2.462045979635577808 ) ) ;
#5686 = AXIS2_PLACEMENT_3D ( 'NONE', #8710, #7461, #3792 ) ;
#5687 = ORIENTED_EDGE ( 'NONE', *, *, #290, .F. ) ;
#5688 = CARTESIAN_POINT ( 'NONE',  ( -5.250000000000000000, -28.93749999931720396, 0.000000000000000000 ) ) ;
#5689 = CARTESIAN_POINT ( 'NONE',  ( 5.114683531249999859, -29.33854166700805877, -2.952963913586932776 ) ) ;
#5690 = ORIENTED_EDGE ( 'NONE', *, *, #97, .T. ) ;
#5691 = AXIS2_PLACEMENT_3D ( 'NONE', #7075, #4884, #7736 ) ;
#5692 = ORIENTED_EDGE ( 'NONE', *, *, #7954, .F. ) ;
#5693 = CARTESIAN_POINT ( 'NONE',  ( -5.385316468750001029, -29.59895833299193413, -3.109213912904136734 ) ) ;
#5694 = CARTESIAN_POINT ( 'NONE',  ( -2.487701488670202910, -7.550659073900639839, -2.462045979635629767 ) ) ;
#5695 = CARTESIAN_POINT ( 'NONE',  ( -1.000000000000000000, -35.00000000000000000, -3.048902179152658931 ) ) ;
#5696 = VERTEX_POINT ( 'NONE', #7581 ) ;
#5697 = CARTESIAN_POINT ( 'NONE',  ( -2.033577675846918216E-14, -29.93750000000000000, 5.250000000000000888 ) ) ;
#5698 = FACE_OUTER_BOUND ( 'NONE', #7995, .T. ) ;
#5699 = EDGE_CURVE ( 'NONE', #1844, #5384, #8960, .T. ) ;
#5700 = CARTESIAN_POINT ( 'NONE',  ( 1.000000000000000000, -29.00000000000000355, -3.048902179152658931 ) ) ;
#5701 = CARTESIAN_POINT ( 'NONE',  ( -5.114683531250000748, -28.73437500034139802, -6.263680815196995234E-16 ) ) ;
#5702 = CARTESIAN_POINT ( 'NONE',  ( 3.507514324621465285, -1.149340926099361226, -1.431606283892619125 ) ) ;
#5703 = CARTESIAN_POINT ( 'NONE',  ( -1.224499502706077880, -6.349340926099361404, -3.007514324621463064 ) ) ;
#5704 = ADVANCED_FACE ( 'NONE', ( #3303 ), #4048, .T. ) ;
#5705 = DIRECTION ( 'NONE',  ( 0.000000000000000000, 1.000000000000000000, 0.000000000000000000 ) ) ;
#5706 = CARTESIAN_POINT ( 'NONE',  ( 5.385316468749999252, -27.46354166632526983, -3.109213912904139399 ) ) ;
#5707 = CARTESIAN_POINT ( 'NONE',  ( -2.815599370228907272, -1.550659073900638507, 2.841254879263473754 ) ) ;
#5708 =( LENGTH_UNIT ( ) NAMED_UNIT ( * ) SI_UNIT ( .MILLI., .METRE. ) );
#5709 = EDGE_CURVE ( 'NONE', #3879, #8139, #2891, .T. ) ;
#5710 = CARTESIAN_POINT ( 'NONE',  ( -1.406733260263393293, -27.70758545099817027, -5.250000000000000000 ) ) ;
#5711 = ORIENTED_EDGE ( 'NONE', *, *, #1617, .F. ) ;
#5712 = SURFACE_STYLE_USAGE ( .BOTH. , #2852 ) ;
#5713 = CARTESIAN_POINT ( 'NONE',  ( -2.625000000000000444, -29.29166666666666785, -4.546633369868303021 ) ) ;
#5714 = ORIENTED_EDGE ( 'NONE', *, *, #6059, .T. ) ;
#5715 = CARTESIAN_POINT ( 'NONE',  ( -5.385316468750000141, -27.57812499965860198, 0.000000000000000000 ) ) ;
#5716 = CARTESIAN_POINT ( 'NONE',  ( 3.007514324621463508, -5.949340926099362825, -1.224499502706076770 ) ) ;
#5717 = ORIENTED_EDGE ( 'NONE', *, *, #1442, .T. ) ;
#5718 = CARTESIAN_POINT ( 'NONE',  ( 2.625000000000000444, -29.20833333333333215, -4.546633369868303021 ) ) ;
#5719 = CARTESIAN_POINT ( 'NONE',  ( 5.249999999999999112, -29.35416666666666430, -3.031088913245536975 ) ) ;
#5720 = CARTESIAN_POINT ( 'NONE',  ( -5.114683531250000748, -27.56770833367473017, -2.952963913586935440 ) ) ;
#5721 = CARTESIAN_POINT ( 'NONE',  ( -5.114683531250000748, -28.29687500034139447, -6.263680815196995234E-16 ) ) ;
#5722 = EDGE_CURVE ( 'NONE', #4375, #6263, #4093, .T. ) ;
#5723 = LINE ( 'NONE', #5166, #5943 ) ;
#5724 = LINE ( 'NONE', #665, #1245 ) ;
#5725 = DIRECTION ( 'NONE',  ( 0.000000000000000000, -1.000000000000000000, 0.000000000000000000 ) ) ;
#5726 = DIRECTION ( 'NONE',  ( 0.000000000000000000, -1.000000000000000000, 0.000000000000000000 ) ) ;
#5727 = CARTESIAN_POINT ( 'NONE',  ( 0.01814118441321408565, -7.849340926099360516, -3.500000000000000000 ) ) ;
#5728 = ADVANCED_FACE ( 'NONE', ( #9011 ), #2614, .T. ) ;
#5729 = ORIENTED_EDGE ( 'NONE', *, *, #2044, .F. ) ;
#5730 = CARTESIAN_POINT ( 'NONE',  ( 1.467888652718972731, -6.650659073900639484, 3.492485675378566246 ) ) ;
#5731 = DIRECTION ( 'NONE',  ( 0.000000000000000000, -1.000000000000000000, 0.000000000000000000 ) ) ;
#5732 = CARTESIAN_POINT ( 'NONE',  ( -5.114683531249999859, -28.50520833367473017, -2.952963913586935440 ) ) ;
#5733 =( BOUNDED_CURVE ( )  B_SPLINE_CURVE ( 2, ( #916, #3764, #5892, #8686, #1712, #6635, #5799, #1665, #4596 ),
 .UNSPECIFIED., .F., .F. ) 
 B_SPLINE_CURVE_WITH_KNOTS ( ( 3, 2, 2, 2, 3 ),
 ( 0.06250000000000000000, 0.06944444444444444753, 0.08333333333333332871, 0.09722222222222222376, 0.1041666666666666713 ),
 .UNSPECIFIED. ) 
 CURVE ( )  GEOMETRIC_REPRESENTATION_ITEM ( )  RATIONAL_B_SPLINE_CURVE ( ( 0.9330127018922194093, 0.9330127018922194093, 1.000000000000000000, 0.8660254037844387076, 1.000000000000000000, 0.8660254037844387076, 1.000000000000000000, 0.9330127018922192983, 0.9330127018922194093 ) ) 
 REPRESENTATION_ITEM ( '' )  );
#5734 = ORIENTED_EDGE ( 'NONE', *, *, #2487, .T. ) ;
#5735 = ORIENTED_EDGE ( 'NONE', *, *, #5766, .T. ) ;
#5736 = CARTESIAN_POINT ( 'NONE',  ( 6.429395695523604153E-16, -30.00000000000000000, -5.250000000000000000 ) ) ;
#5737 = CARTESIAN_POINT ( 'NONE',  ( 4.007514324621432422, -0.4506590739006384738, 1.638713065079246078 ) ) ;
#5738 = CARTESIAN_POINT ( 'NONE',  ( 2.143131898507868051E-16, -53.00000000000000000, -1.749999999999999778 ) ) ;
#5739 = ORIENTED_EDGE ( 'NONE', *, *, #2369, .T. ) ;
#5740 = CARTESIAN_POINT ( 'NONE',  ( -1.975475456537005874E-15, -27.56249999999999289, 5.250000000000000000 ) ) ;
#5741 = DIRECTION ( 'NONE',  ( 0.000000000000000000, -1.000000000000000000, 0.000000000000000000 ) ) ;
#5742 = STYLED_ITEM ( 'NONE', ( #5212 ), #4641 ) ;
#5743 = CONICAL_SURFACE ( 'NONE', #2812, 2.750000000000000000, 0.08726646259971666819 ) ;
#5744 = CARTESIAN_POINT ( 'NONE',  ( 2.625000000000002220, -27.35416666598386826, 4.546633369868302132 ) ) ;
#5745 = CARTESIAN_POINT ( 'NONE',  ( 5.114683531249999859, -27.83854166700806587, -2.952963913586932776 ) ) ;
#5746 = CARTESIAN_POINT ( 'NONE',  ( 0.000000000000000000, -27.00000000000000000, 0.000000000000000000 ) ) ;
#5747 = ITEM_DEFINED_TRANSFORMATION ( 'NONE', 'NONE', #6206,  #888 ) ;
#5748 = CARTESIAN_POINT ( 'NONE',  ( 1.185285273922203525E-14, -28.96875000068279959, -5.250000000000000000 ) ) ;
#5749 = CARTESIAN_POINT ( 'NONE',  ( -2.108492589042306964, -6.449340926099361049, -2.134148098076978251 ) ) ;
#5750 = CARTESIAN_POINT ( 'NONE',  ( -5.250000000000000888, -28.13541666734947100, 3.031088913245533423 ) ) ;
#5751 = PRODUCT_DEFINITION_FORMATION_WITH_SPECIFIED_SOURCE ( 'ANY', '', #691, .NOT_KNOWN. ) ;
#5752 = CARTESIAN_POINT ( 'NONE',  ( -3.807688866302469071E-16, -28.42187499965859843, -6.218427825808274356 ) ) ;
#5753 = CARTESIAN_POINT ( 'NONE',  ( -2.841254879263533262, -3.649340926099360782, 2.815599370228847764 ) ) ;
#5754 = DIRECTION ( 'NONE',  ( 0.000000000000000000, 1.000000000000000000, 0.000000000000000000 ) ) ;
#5755 = DIRECTION ( 'NONE',  ( 1.039441819132096507E-14, 0.07256473765270715637, -0.9973637043974449279 ) ) ;
#5756 = EDGE_CURVE ( 'NONE', #5029, #4261, #3336, .T. ) ;
#5757 = ORIENTED_EDGE ( 'NONE', *, *, #2827, .T. ) ;
#5758 = CARTESIAN_POINT ( 'NONE',  ( 5.250000000000000000, -29.62500000000000000, -6.429395695523604153E-16 ) ) ;
#5759 = ORIENTED_EDGE ( 'NONE', *, *, #546, .F. ) ;
#5760 = CARTESIAN_POINT ( 'NONE',  ( -5.385316468750000141, -27.07812499965860198, 0.000000000000000000 ) ) ;
#5761 = CARTESIAN_POINT ( 'NONE',  ( -0.01814118441314477650, -7.350659073900640550, -3.000000000000000444 ) ) ;
#5762 = ORIENTED_EDGE ( 'NONE', *, *, #2090, .F. ) ;
#5763 = CARTESIAN_POINT ( 'NONE',  ( 2.624999999999996891, -28.54166666666666785, 4.546633369868304797 ) ) ;
#5764 = VECTOR ( 'NONE', #2723, 1000.000000000000000 ) ;
#5765 = CARTESIAN_POINT ( 'NONE',  ( -2.557341765624999042, -27.33854166700806587, -4.429445870380400052 ) ) ;
#5766 = EDGE_CURVE ( 'NONE', #6114, #2260, #4001, .T. ) ;
#5767 = CIRCLE ( 'NONE', #8164, 5.250000000000000000 ) ;
#5768 = CARTESIAN_POINT ( 'NONE',  ( 5.114683531250000748, -27.67187500034139802, 0.000000000000000000 ) ) ;
#5769 = CARTESIAN_POINT ( 'NONE',  ( 0.000000000000000000, 75.00000000000000000, 0.000000000000000000 ) ) ;
#5770 = DIRECTION ( 'NONE',  ( 0.8660254037844402619, -0.4999999999999970579, 0.000000000000000000 ) ) ;
#5771 = CARTESIAN_POINT ( 'NONE',  ( 9.180150650966086169E-15, -28.56249999999999645, 5.249999999999999112 ) ) ;
#5772 = PLANE ( 'NONE',  #6282 ) ;
#5773 = CARTESIAN_POINT ( 'NONE',  ( -2.557341765624999042, -29.58854166700806232, -4.429445870380400052 ) ) ;
#5774 = FILL_AREA_STYLE_COLOUR ( '', #3026 ) ;
#5775 = VERTEX_POINT ( 'NONE', #8964 ) ;
#5776 = AXIS2_PLACEMENT_3D ( 'NONE', #2531, #1085, #5355 ) ;
#5777 = CARTESIAN_POINT ( 'NONE',  ( -2.487701488670202910, -5.950659073900639306, -2.462045979635629767 ) ) ;
#5778 = DIRECTION ( 'NONE',  ( 0.000000000000000000, 0.000000000000000000, -1.000000000000000000 ) ) ;
#5779 = CARTESIAN_POINT ( 'NONE',  ( -5.114683531249999859, -28.25520833367473017, -2.952963913586935440 ) ) ;
#5780 = ORIENTED_EDGE ( 'NONE', *, *, #6043, .T. ) ;
#5781 = EDGE_LOOP ( 'NONE', ( #3475, #4611 ) ) ;
#5782 = AXIS2_PLACEMENT_3D ( 'NONE', #7174, #6466, #8059 ) ;
#5783 = CARTESIAN_POINT ( 'NONE',  ( 6.972266317189433020E-16, -28.68749999999999645, -5.249999999999999112 ) ) ;
#5784 = CARTESIAN_POINT ( 'NONE',  ( 2.033577675846918216E-14, -26.84375000068279959, 5.250000000000000888 ) ) ;
#5785 = CARTESIAN_POINT ( 'NONE',  ( 0.01814118441313467001, -4.950659073900639306, 4.000000000000000000 ) ) ;
#5786 = FACE_OUTER_BOUND ( 'NONE', #8623, .T. ) ;
#5787 = EDGE_LOOP ( 'NONE', ( #6426, #7090, #1216, #1048 ) ) ;
#5788 = AXIS2_PLACEMENT_3D ( 'NONE', #3441, #7528, #2040 ) ;
#5789 =( BOUNDED_CURVE ( )  B_SPLINE_CURVE ( 2, ( #3682, #6505, #141, #2993, #8654, #6079, #4601, #1156, #1255 ),
 .UNSPECIFIED., .F., .F. ) 
 B_SPLINE_CURVE_WITH_KNOTS ( ( 3, 2, 2, 2, 3 ),
 ( 0.06250000000000000000, 0.06944444444444444753, 0.08333333333333332871, 0.09722222222222222376, 0.1041666666666666713 ),
 .UNSPECIFIED. ) 
 CURVE ( )  GEOMETRIC_REPRESENTATION_ITEM ( )  RATIONAL_B_SPLINE_CURVE ( ( 0.9330127018922194093, 0.9330127018922194093, 1.000000000000000000, 0.8660254037844387076, 1.000000000000000000, 0.8660254037844387076, 1.000000000000000000, 0.9330127018922192983, 0.9330127018922194093 ) ) 
 REPRESENTATION_ITEM ( '' )  );
#5790 = DIRECTION ( 'NONE',  ( -0.000000000000000000, -1.000000000000000000, -0.000000000000000000 ) ) ;
#5791 = CARTESIAN_POINT ( 'NONE',  ( -2.624999999999998668, -28.94791666734946389, -4.546633369868303021 ) ) ;
#5792 = DIRECTION ( 'NONE',  ( 0.000000000000000000, 0.000000000000000000, -1.000000000000000000 ) ) ;
#5793 = UNCERTAINTY_MEASURE_WITH_UNIT (LENGTH_MEASURE( 1.000000000000000082E-05 ), #3922, 'distance_accuracy_value', 'NONE');
#5794 = CARTESIAN_POINT ( 'NONE',  ( 5.114683531249999859, -27.58854166700806587, -2.952963913586932776 ) ) ;
#5795 = CARTESIAN_POINT ( 'NONE',  ( 0.000000000000000000, -27.00000000000000000, 0.000000000000000000 ) ) ;
#5796 = CIRCLE ( 'NONE', #1800, 3.794308781941904574 ) ;
#5797 = DIRECTION ( 'NONE',  ( 0.000000000000000000, 1.000000000000000000, 0.000000000000000000 ) ) ;
#5798 = CARTESIAN_POINT ( 'NONE',  ( 2.134148098076978251, -6.049340926099361582, -2.108492589042307408 ) ) ;
#5799 = CARTESIAN_POINT ( 'NONE',  ( -2.625000000000000444, -27.47916666598386826, -4.546633369868303021 ) ) ;
#5800 = ADVANCED_FACE ( 'NONE', ( #510 ), #4793, .T. ) ;
#5801 = CARTESIAN_POINT ( 'NONE',  ( -1.674995433905516196, -7.450659073900640195, -3.992485675378566690 ) ) ;
#5802 = CARTESIAN_POINT ( 'NONE',  ( 2.625000000000002220, -28.35416666598386826, 4.546633369868302132 ) ) ;
#5803 = AXIS2_PLACEMENT_3D ( 'NONE', #3350, #551, #6180 ) ;
#5804 = CARTESIAN_POINT ( 'NONE',  ( 0.000000000000000000, -28.00000000000000000, 0.000000000000000000 ) ) ;
#5805 = CARTESIAN_POINT ( 'NONE',  ( -5.250000000000000888, -27.85416666666666430, 3.031088913245533423 ) ) ;
#5806 = PRODUCT_RELATED_PRODUCT_CATEGORY ( 'part', '', ( #4597 ) ) ;
#5807 = CARTESIAN_POINT ( 'NONE',  ( 0.000000000000000000, -46.00000000000000000, 1.750000000000000222 ) ) ;
#5808 = ORIENTED_EDGE ( 'NONE', *, *, #8122, .F. ) ;
#5809 = CARTESIAN_POINT ( 'NONE',  ( 5.385316468750001029, -28.72395833299193413, 3.109213912904135846 ) ) ;
#5810 = CARTESIAN_POINT ( 'NONE',  ( 1.975475456537005874E-15, -28.68749999999999645, 5.250000000000000000 ) ) ;
#5811 = EDGE_LOOP ( 'NONE', ( #1757, #4853, #6362, #8676 ) ) ;
#5812 = CARTESIAN_POINT ( 'NONE',  ( -2.692658234374996518, -27.28645833299193413, 4.663820869356208654 ) ) ;
#5813 = CARTESIAN_POINT ( 'NONE',  ( 3.007514324621436863, -3.650659073900639928, 1.224499502706140719 ) ) ;
#5814 = ORIENTED_EDGE ( 'NONE', *, *, #5917, .F. ) ;
#5815 = CARTESIAN_POINT ( 'NONE',  ( 5.249999999999999112, -28.77083333333333215, 3.031088913245538308 ) ) ;
#5816 = CARTESIAN_POINT ( 'NONE',  ( 0.000000000000000000, 69.99999999999998579, 0.000000000000000000 ) ) ;
#5817 = CARTESIAN_POINT ( 'NONE',  ( -1.084901341431563726E-15, -28.48437500034139802, 5.905927827173866440 ) ) ;
#5818 =( LENGTH_UNIT ( ) NAMED_UNIT ( * ) SI_UNIT ( .MILLI., .METRE. ) );
#5819 = CARTESIAN_POINT ( 'NONE',  ( -5.114683531250000748, -27.77604166700806587, 2.952963913586931888 ) ) ;
#5820 = DIRECTION ( 'NONE',  ( -0.000000000000000000, -1.000000000000000000, -0.000000000000000000 ) ) ;
#5821 = CARTESIAN_POINT ( 'NONE',  ( 3.507514324621465285, -5.949340926099361937, -1.431606283892619125 ) ) ;
#5822 = DIRECTION ( 'NONE',  ( 0.000000000000000000, 1.000000000000000000, 0.000000000000000000 ) ) ;
#5823 = CARTESIAN_POINT ( 'NONE',  ( 1.045839947578414884E-14, -28.06249999999999289, -5.249999999999999112 ) ) ;
#5824 = SURFACE_STYLE_FILL_AREA ( #2341 ) ;
#5825 = AXIS2_PLACEMENT_3D ( 'NONE', #1380, #8457, #2082 ) ;
#5826 = VERTEX_POINT ( 'NONE', #2334 ) ;
#5827 = CARTESIAN_POINT ( 'NONE',  ( -3.500000000000000000, -6.150659073900639484, 0.01814118441314012051 ) ) ;
#5828 = AXIS2_PLACEMENT_3D ( 'NONE', #2290, #3786, #6610 ) ;
#5829 = CARTESIAN_POINT ( 'NONE',  ( -5.249999999999999112, -29.39583333333332860, -3.031088913245536975 ) ) ;
#5830 = CARTESIAN_POINT ( 'NONE',  ( -5.114683531250000748, -28.48437500034139802, -6.263680815196995234E-16 ) ) ;
#5831 = EDGE_CURVE ( 'NONE', #3312, #3105, #37, .T. ) ;
#5832 = ORIENTED_EDGE ( 'NONE', *, *, #1888, .F. ) ;
#5833 = CARTESIAN_POINT ( 'NONE',  ( 2.033577675846918216E-14, -27.09375000068279604, 5.250000000000000888 ) ) ;
#5834 = CARTESIAN_POINT ( 'NONE',  ( -5.385316468750001029, -27.63020833299193768, -3.109213912904136734 ) ) ;
#5835 = CARTESIAN_POINT ( 'NONE',  ( 4.007514324621432422, -5.250659073900638241, 1.638713065079246078 ) ) ;
#5836 = AXIS2_PLACEMENT_3D ( 'NONE', #2720, #7553, #5502 ) ;
#5837 = CARTESIAN_POINT ( 'NONE',  ( 0.000000000000000000, 70.00000000000000000, -1.500000000000000222 ) ) ;
#5838 = ORIENTED_EDGE ( 'NONE', *, *, #3174, .F. ) ;
#5839 = CARTESIAN_POINT ( 'NONE',  ( 0.000000000000000000, 70.00000000000000000, 0.000000000000000000 ) ) ;
#5840 = CARTESIAN_POINT ( 'NONE',  ( 2.624999999999996891, -29.57291666734946034, 4.546633369868304797 ) ) ;
#5841 = CARTESIAN_POINT ( 'NONE',  ( 2.692658234374998738, -28.19270833299193413, -4.663820869356206877 ) ) ;
#5842 = AXIS2_PLACEMENT_3D ( 'NONE', #2972, #3070, #7380 ) ;
#5843 = CARTESIAN_POINT ( 'NONE',  ( 2.557341765625000818, -29.88020833367473372, -4.429445870380400052 ) ) ;
#5844 = DIRECTION ( 'NONE',  ( 0.000000000000000000, -0.000000000000000000, 1.000000000000000000 ) ) ;
#5845 = CARTESIAN_POINT ( 'NONE',  ( 2.992485675378565357, -2.250659073900640461, -1.260781871532430376 ) ) ;
#5846 = CYLINDRICAL_SURFACE ( 'NONE', #1620, 5.250000000000000000 ) ;
#5847 = CARTESIAN_POINT ( 'NONE',  ( -1.674995433905599462, -2.149340926099360782, 3.992485675378533383 ) ) ;
#5848 = AXIS2_PLACEMENT_3D ( 'NONE', #8765, #2396, #2208 ) ;
#5849 = CARTESIAN_POINT ( 'NONE',  ( -2.624999999999996891, -28.39583333265053611, 4.546633369868304797 ) ) ;
#5850 = CARTESIAN_POINT ( 'NONE',  ( 6.972266317189433020E-16, -27.18750000000000000, -5.249999999999999112 ) ) ;
#5851 = CARTESIAN_POINT ( 'NONE',  ( 3.492485675378535603, -5.749340926099362648, 1.467888652719046672 ) ) ;
#5852 = DIRECTION ( 'NONE',  ( 0.000000000000000000, -0.9961946980917455452, -0.08715574274765836016 ) ) ;
#5853 = EDGE_LOOP ( 'NONE', ( #7431, #8166 ) ) ;
#5854 = CARTESIAN_POINT ( 'NONE',  ( 2.692658234374998738, -27.66145833299193413, -4.663820869356206877 ) ) ;
#5855 = CARTESIAN_POINT ( 'NONE',  ( -4.007514324621467949, -6.749340926099361759, 1.638713065079161924 ) ) ;
#5856 = CARTESIAN_POINT ( 'NONE',  ( -1.406733260263385521, -27.32366454968462932, 5.250000000000006217 ) ) ;
#5857 = ORIENTED_EDGE ( 'NONE', *, *, #2944, .F. ) ;
#5858 = CARTESIAN_POINT ( 'NONE',  ( 2.692658234374998738, -27.41145833299193413, -4.663820869356206877 ) ) ;
#5859 = CARTESIAN_POINT ( 'NONE',  ( -3.007514324621435531, -6.050659073900639839, -1.224499502706142273 ) ) ;
#5860 = ORIENTED_EDGE ( 'NONE', *, *, #1586, .T. ) ;
#5861 = CARTESIAN_POINT ( 'NONE',  ( 5.250000000000000000, -28.22916666666666430, -3.031088913245534755 ) ) ;
#5862 = CARTESIAN_POINT ( 'NONE',  ( -2.557341765624999042, -28.08854166700806587, -4.429445870380400052 ) ) ;
#5863 = FILL_AREA_STYLE_COLOUR ( '', #1299 ) ;
#5864 = PLANE ( 'NONE',  #6294 ) ;
#5865 = DIRECTION ( 'NONE',  ( 0.000000000000000000, -0.9975640502598241977, -0.06975647374412545509 ) ) ;
#5866 = CARTESIAN_POINT ( 'NONE',  ( -0.01814118441321365544, -2.249340926099361315, 3.500000000000000000 ) ) ;
#5867 = CARTESIAN_POINT ( 'NONE',  ( 0.000000000000000000, -30.00000000000000000, 0.000000000000000000 ) ) ;
#5868 = DIRECTION ( 'NONE',  ( 0.000000000000000000, 0.000000000000000000, 1.000000000000000000 ) ) ;
#5869 = CARTESIAN_POINT ( 'NONE',  ( 3.507514324621465285, -7.549340926099362470, -1.431606283892619125 ) ) ;
#5870 =( BOUNDED_CURVE ( )  B_SPLINE_CURVE ( 2, ( #5268, #7414, #8114, #2488, #6108, #8936, #8162, #3887, #2588 ),
 .UNSPECIFIED., .F., .T. ) 
 B_SPLINE_CURVE_WITH_KNOTS ( ( 3, 2, 2, 2, 3 ),
 ( 0.2291666666666666574, 0.2361111111111111049, 0.2500000000000000000, 0.2638888888888888951, 0.2708333333333333148 ),
 .UNSPECIFIED. ) 
 CURVE ( )  GEOMETRIC_REPRESENTATION_ITEM ( )  RATIONAL_B_SPLINE_CURVE ( ( 0.9330127018922194093, 0.9330127018922194093, 1.000000000000000000, 0.8660254037844387076, 1.000000000000000000, 0.8660254037844387076, 1.000000000000000000, 0.9330127018922196314, 0.9330127018922194093 ) ) 
 REPRESENTATION_ITEM ( '' )  );
#5871 = CARTESIAN_POINT ( 'NONE',  ( 2.625000000000000444, -27.23958333401612819, -4.546633369868303021 ) ) ;
#5872 = ADVANCED_FACE ( 'NONE', ( #2479, #8104 ), #5864, .F. ) ;
#5873 = ORIENTED_EDGE ( 'NONE', *, *, #6326, .F. ) ;
#5874 = CARTESIAN_POINT ( 'NONE',  ( 5.249999999999999112, -27.10416666666666430, -3.031088913245536975 ) ) ;
#5875 = CARTESIAN_POINT ( 'NONE',  ( -1.975475456537005874E-15, -29.31250000000000000, 5.250000000000000000 ) ) ;
#5876 = CARTESIAN_POINT ( 'NONE',  ( -5.114683531250000748, -27.98437500034139802, -6.263680815196995234E-16 ) ) ;
#5877 = ORIENTED_EDGE ( 'NONE', *, *, #6896, .T. ) ;
#5878 = ADVANCED_FACE ( 'NONE', ( #377 ), #1639, .T. ) ;
#5879 = CARTESIAN_POINT ( 'NONE',  ( -5.250000000000000000, -29.75000000000000000, 0.000000000000000000 ) ) ;
#5880 = CARTESIAN_POINT ( 'NONE',  ( 2.692658234375002735, -28.02604166632526628, 4.663820869356205101 ) ) ;
#5881 = CARTESIAN_POINT ( 'NONE',  ( -3.992485675378568022, -4.650659073900640372, 1.674995433905515529 ) ) ;
#5882 = CARTESIAN_POINT ( 'NONE',  ( 5.249999999999999112, -27.47916666666666430, -3.031088913245534755 ) ) ;
#5883 = ORIENTED_EDGE ( 'NONE', *, *, #2778, .T. ) ;
#5884 = CARTESIAN_POINT ( 'NONE',  ( 0.000000000000000000, 81.00000000000001421, -4.000000000000000000 ) ) ;
#5885 = CARTESIAN_POINT ( 'NONE',  ( -5.250000000000000000, -28.90625000068279604, -6.429395695523604153E-16 ) ) ;
#5886 = CARTESIAN_POINT ( 'NONE',  ( 2.692658234375002735, -28.02604166632526628, 4.663820869356205101 ) ) ;
#5887 = CARTESIAN_POINT ( 'NONE',  ( -1.084901341431563923E-15, -26.92187500034139802, 5.905927827173866440 ) ) ;
#5888 = DIRECTION ( 'NONE',  ( 0.000000000000000000, 1.000000000000000000, 0.000000000000000000 ) ) ;
#5889 = CARTESIAN_POINT ( 'NONE',  ( 5.250000000000000888, -28.83333333265053966, 3.031088913245533423 ) ) ;
#5890 = CARTESIAN_POINT ( 'NONE',  ( 0.01814118441314514080, -1.750659073900639351, 3.000000000000000444 ) ) ;
#5891 = UNCERTAINTY_MEASURE_WITH_UNIT (LENGTH_MEASURE( 1.000000000000000082E-05 ), #6946, 'distance_accuracy_value', 'NONE');
#5892 = CARTESIAN_POINT ( 'NONE',  ( -2.624999999999996891, -27.39583333265053611, 4.546633369868304797 ) ) ;
#5893 = CARTESIAN_POINT ( 'NONE',  ( -3.992485675378532939, -1.749340926099360871, -1.674995433905601683 ) ) ;
#5894 = CARTESIAN_POINT ( 'NONE',  ( -3.712013335537174572E-16, -28.24999999931720041, -6.062177826491070398 ) ) ;
#5895 = LINE ( 'NONE', #3812, #5682 ) ;
#5896 = CARTESIAN_POINT ( 'NONE',  ( 3.507514324621465285, -4.349340926099361404, -1.431606283892619347 ) ) ;
#5897 = CARTESIAN_POINT ( 'NONE',  ( -1.000000000000000000, -35.00000000000000000, -3.048902179152658931 ) ) ;
#5898 = PRESENTATION_LAYER_ASSIGNMENT (  '', '', ( #9023 ) ) ;
#5899 = CARTESIAN_POINT ( 'NONE',  ( 2.692658234374998738, -28.41145833299193413, -4.663820869356206877 ) ) ;
#5900 = EDGE_CURVE ( 'NONE', #6843, #1752, #54, .T. ) ;
#5901 = CARTESIAN_POINT ( 'NONE',  ( 4.007514324621469726, -4.349340926099361404, -1.638713065079161257 ) ) ;
#5902 = CARTESIAN_POINT ( 'NONE',  ( -5.249999999999999112, -27.39583333333333215, -3.031088913245536975 ) ) ;
#5903 = EDGE_LOOP ( 'NONE', ( #9174, #4737 ) ) ;
#5904 = CARTESIAN_POINT ( 'NONE',  ( -2.692658234375000514, -27.36979166632526628, -4.663820869356205989 ) ) ;
#5905 = CARTESIAN_POINT ( 'NONE',  ( -3.000000000000000444, -6.150659073900639484, 0.01814118441314532468 ) ) ;
#5906 = EDGE_LOOP ( 'NONE', ( #5122, #1727, #3834, #1026 ) ) ;
#5907 = CARTESIAN_POINT ( 'NONE',  ( 2.625000000000000444, -27.20833333333333215, -4.546633369868303021 ) ) ;
#5908 =( GEOMETRIC_REPRESENTATION_CONTEXT ( 3 ) GLOBAL_UNCERTAINTY_ASSIGNED_CONTEXT ( ( #1516 ) ) GLOBAL_UNIT_ASSIGNED_CONTEXT ( ( #2714, #6098, #6983 ) ) REPRESENTATION_CONTEXT ( 'NONE', 'WORKASPACE' ) );
#5909 = CARTESIAN_POINT ( 'NONE',  ( 2.557341765625000818, -27.63020833367473017, -4.429445870380400052 ) ) ;
#5910 = DIRECTION ( 'NONE',  ( 1.000000000000000000, 0.000000000000000000, 0.000000000000000000 ) ) ;
#5911 = CARTESIAN_POINT ( 'NONE',  ( 5.114683531249998971, -26.94270833367472662, 2.952963913586936329 ) ) ;
#5912 = CARTESIAN_POINT ( 'NONE',  ( -5.249999999999999112, -29.91666666598387181, 3.031088913245538308 ) ) ;
#5913 = CARTESIAN_POINT ( 'NONE',  ( 1.431606283892619125, -0.7493409260993610932, 3.507514324621464397 ) ) ;
#5914 = PLANE ( 'NONE',  #7123 ) ;
#5915 = LINE ( 'NONE', #3144, #1524 ) ;
#5916 = CARTESIAN_POINT ( 'NONE',  ( -2.557341765625002594, -28.25520833367473017, 4.429445870380399164 ) ) ;
#5917 = EDGE_CURVE ( 'NONE', #3802, #7275, #8236, .T. ) ;
#5918 = ORIENTED_EDGE ( 'NONE', *, *, #6113, .T. ) ;
#5919 = CARTESIAN_POINT ( 'NONE',  ( -5.250000000000000000, -30.00000000000000000, 0.000000000000000000 ) ) ;
#5920 = CARTESIAN_POINT ( 'NONE',  ( 3.616337804771879580E-16, -28.29687500034139802, -5.905927827173866440 ) ) ;
#5921 = AXIS2_PLACEMENT_3D ( 'NONE', #7535, #1873, #1298 ) ;
#5922 = PRODUCT_DEFINITION_SHAPE ( 'NONE', 'NONE',  #9192 ) ;
#5923 = EDGE_LOOP ( 'NONE', ( #9154, #1768, #7664, #835 ) ) ;
#5924 =( BOUNDED_CURVE ( )  B_SPLINE_CURVE ( 2, ( #106, #374, #4392, #5874, #3919, #846, #3694, #3005, #8667 ),
 .UNSPECIFIED., .F., .F. ) 
 B_SPLINE_CURVE_WITH_KNOTS ( ( 3, 2, 2, 2, 3 ),
 ( 0.02083333333333333218, 0.02777777777777777624, 0.04166666666666666435, 0.05555555555555555247, 0.06250000000000000000 ),
 .UNSPECIFIED. ) 
 CURVE ( )  GEOMETRIC_REPRESENTATION_ITEM ( )  RATIONAL_B_SPLINE_CURVE ( ( 0.9330127018922194093, 0.9330127018922194093, 1.000000000000000000, 0.8660254037844387076, 1.000000000000000000, 0.8660254037844387076, 1.000000000000000000, 0.9330127018922194093, 0.9330127018922194093 ) ) 
 REPRESENTATION_ITEM ( '' )  );
#5925 = FACE_OUTER_BOUND ( 'NONE', #1656, .T. ) ;
#5926 = CARTESIAN_POINT ( 'NONE',  ( 0.000000000000000000, -30.00000000000000000, 5.250000000000000000 ) ) ;
#5927 = CARTESIAN_POINT ( 'NONE',  ( -4.000000000000000000, -6.150659073900637708, 0.01814118441313491634 ) ) ;
#5928 = CARTESIAN_POINT ( 'NONE',  ( -5.250000000000000000, -29.12499999999999645, -6.429395695523604153E-16 ) ) ;
#5929 = CARTESIAN_POINT ( 'NONE',  ( 5.385316468750001029, -27.75520833299194123, 3.109213912904135846 ) ) ;
#5930 = ORIENTED_EDGE ( 'NONE', *, *, #5548, .T. ) ;
#5931 = FACE_OUTER_BOUND ( 'NONE', #3127, .T. ) ;
#5932 = CARTESIAN_POINT ( 'NONE',  ( -5.250000000000000888, -29.13541666734946389, 3.031088913245532979 ) ) ;
#5933 = CARTESIAN_POINT ( 'NONE',  ( 5.385316468750000141, -28.23437499965860198, -6.595110575850215044E-16 ) ) ;
#5934 = AXIS2_PLACEMENT_3D ( 'NONE', #8855, #4631, #3288 ) ;
#5935 = CARTESIAN_POINT ( 'NONE',  ( 3.616337804771879580E-16, -27.79687500034139802, -5.905927827173866440 ) ) ;
#5936 = ORIENTED_EDGE ( 'NONE', *, *, #79, .T. ) ;
#5937 = CARTESIAN_POINT ( 'NONE',  ( 0.000000000000000000, -30.00000000000000000, 0.000000000000000000 ) ) ;
#5938 = CARTESIAN_POINT ( 'NONE',  ( 3.000000000000000444, -5.350659073900639662, -0.01814118441314496039 ) ) ;
#5939 = LINE ( 'NONE', #8779, #8752 ) ;
#5940 = CARTESIAN_POINT ( 'NONE',  ( 5.250000000000000888, -28.08333333265053255, 3.031088913245532979 ) ) ;
#5941 = DIRECTION ( 'NONE',  ( 0.000000000000000000, 0.000000000000000000, -1.000000000000000000 ) ) ;
#5942 = CARTESIAN_POINT ( 'NONE',  ( -0.01814118441321365544, -2.249340926099361315, 3.500000000000000000 ) ) ;
#5943 = VECTOR ( 'NONE', #3594, 1000.000000000000000 ) ;
#5944 = EDGE_CURVE ( 'NONE', #7114, #3963, #1291, .T. ) ;
#5945 = LINE ( 'NONE', #5102, #450 ) ;
#5946 = CARTESIAN_POINT ( 'NONE',  ( 0.000000000000000000, -30.00000000000000000, 0.000000000000000000 ) ) ;
#5947 = CARTESIAN_POINT ( 'NONE',  ( 0.000000000000000000, 0.000000000000000000, 0.000000000000000000 ) ) ;
#5948 = CARTESIAN_POINT ( 'NONE',  ( -5.385316468749998364, -27.55729166632526628, 3.109213912904140287 ) ) ;
#5949 = CARTESIAN_POINT ( 'NONE',  ( 2.815599370228847320, -7.249340926099360871, 2.841254879263533262 ) ) ;
#5950 = CARTESIAN_POINT ( 'NONE',  ( -2.625000000000000444, -28.54166666666666785, -4.546633369868303021 ) ) ;
#5951 = VERTEX_POINT ( 'NONE', #5572 ) ;
#5952 = CARTESIAN_POINT ( 'NONE',  ( 2.692658234375002735, -28.99479166632526983, 4.663820869356205101 ) ) ;
#5953 = CARTESIAN_POINT ( 'NONE',  ( -2.992485675378564469, -6.250659073900639129, 1.260781871532430820 ) ) ;
#5954 = ORIENTED_EDGE ( 'NONE', *, *, #5588, .T. ) ;
#5955 = CARTESIAN_POINT ( 'NONE',  ( -2.625000000000002220, -27.58333333333333215, 4.546633369868302132 ) ) ;
#5956 = CARTESIAN_POINT ( 'NONE',  ( 1.467888652718972731, -0.2506590739006389623, 3.492485675378566246 ) ) ;
#5957 = VERTEX_POINT ( 'NONE', #7060 ) ;
#5958 =( NAMED_UNIT ( * ) PLANE_ANGLE_UNIT ( ) SI_UNIT ( $, .RADIAN. ) );
#5959 = CARTESIAN_POINT ( 'NONE',  ( -2.624999999999996891, -27.70833333333333215, 4.546633369868304797 ) ) ;
#5960 = VERTEX_POINT ( 'NONE', #1296 ) ;
#5961 = CARTESIAN_POINT ( 'NONE',  ( -5.114683531250000748, -28.48437500034139802, -6.263680815196995234E-16 ) ) ;
#5962 = CARTESIAN_POINT ( 'NONE',  ( 1.431606283892619125, -3.949340926099361049, 3.507514324621464397 ) ) ;
#5963 = CARTESIAN_POINT ( 'NONE',  ( 5.249999999999999112, -28.51041666734946389, -3.031088913245534755 ) ) ;
#5964 = CARTESIAN_POINT ( 'NONE',  ( -1.406733260263382856, -27.45758545099817027, -5.250000000000006217 ) ) ;
#5965 = CARTESIAN_POINT ( 'NONE',  ( -5.114683531249999859, -29.31770833367473372, -2.952963913586935440 ) ) ;
#5966 = ORIENTED_EDGE ( 'NONE', *, *, #7534, .T. ) ;
#5967 = CARTESIAN_POINT ( 'NONE',  ( -1.920924113947233058, -1.125130374610751609E-16, 2.915376471134273118 ) ) ;
#5968 = ORIENTED_EDGE ( 'NONE', *, *, #3959, .F. ) ;
#5969 = DIRECTION ( 'NONE',  ( 0.000000000000000000, 0.000000000000000000, -1.000000000000000000 ) ) ;
#5970 = CARTESIAN_POINT ( 'NONE',  ( -3.807688866302469071E-16, -27.17187499965860198, -6.218427825808274356 ) ) ;
#5971 = CARTESIAN_POINT ( 'NONE',  ( 1.638713065079247855, -4.050659073900639839, -4.007514324621431534 ) ) ;
#5972 = CARTESIAN_POINT ( 'NONE',  ( 2.692658234375002735, -27.52604166632526628, 4.663820869356205101 ) ) ;
#5973 = ORIENTED_EDGE ( 'NONE', *, *, #6142, .T. ) ;
#5974 = DIRECTION ( 'NONE',  ( -1.492469013153037857E-17, 0.9925461516413219831, 0.1218693434051477398 ) ) ;
#5975 = DIRECTION ( 'NONE',  ( 1.000000000000000000, 0.000000000000000000, 0.000000000000000000 ) ) ;
#5976 = CARTESIAN_POINT ( 'NONE',  ( 2.692658234374998738, -28.44270833299193413, -4.663820869356206877 ) ) ;
#5977 = CIRCLE ( 'NONE', #1990, 3.999999999999999112 ) ;
#5978 = CIRCLE ( 'NONE', #1984, 6.250000000000000000 ) ;
#5979 = EDGE_LOOP ( 'NONE', ( #3155, #3321, #6412, #7752 ) ) ;
#5980 = FACE_BOUND ( 'NONE', #212, .T. ) ;
#5981 = CARTESIAN_POINT ( 'NONE',  ( -1.224499502706077880, -7.949340926099362825, -3.007514324621463064 ) ) ;
#5982 = CARTESIAN_POINT ( 'NONE',  ( -2.624999999999996891, -29.39583333265053611, 4.546633369868304797 ) ) ;
#5983 = EDGE_CURVE ( 'NONE', #3304, #5172, #1539, .T. ) ;
#5984=STYLED_ITEM('',(#9218),#5133);
#5985 = CARTESIAN_POINT ( 'NONE',  ( 5.250000000000000000, -28.56249999931720396, -6.429395695523604153E-16 ) ) ;
#5986 = DIRECTION ( 'NONE',  ( 1.000000000000000000, -0.000000000000000000, 1.047711134623677467E-14 ) ) ;
#5987 = CARTESIAN_POINT ( 'NONE',  ( -3.500000000000000000, -5.049340926099361582, -0.01814118441321344033 ) ) ;
#5988 = EDGE_CURVE ( 'NONE', #8128, #8745, #3252, .T. ) ;
#5989 = CARTESIAN_POINT ( 'NONE',  ( 5.250000000000000000, -29.56249999931720041, -6.429395695523604153E-16 ) ) ;
#5990 = ORIENTED_EDGE ( 'NONE', *, *, #4524, .F. ) ;
#5991 = DIRECTION ( 'NONE',  ( 0.000000000000000000, 0.000000000000000000, 1.000000000000000000 ) ) ;
#5992 = CARTESIAN_POINT ( 'NONE',  ( 5.385316468750001029, -28.22395833299193058, 3.109213912904135846 ) ) ;
#5993 = CARTESIAN_POINT ( 'NONE',  ( 1.638713065079161924, -5.549340926099361582, 4.007514324621467949 ) ) ;
#5994 = CIRCLE ( 'NONE', #7783, 2.549999999999999822 ) ;
#5995 = ORIENTED_EDGE ( 'NONE', *, *, #5260, .F. ) ;
#5996 = CARTESIAN_POINT ( 'NONE',  ( 5.385316468750000141, -28.20312499965860198, -6.595110575850215044E-16 ) ) ;
#5997 = CARTESIAN_POINT ( 'NONE',  ( 2.462045979635629767, -5.550659073900639839, -2.487701488670203354 ) ) ;
#5998 = ORIENTED_EDGE ( 'NONE', *, *, #4871, .F. ) ;
#5999 = CARTESIAN_POINT ( 'NONE',  ( -5.250000000000000000, -28.39583333333333215, -3.031088913245536531 ) ) ;
#6000 = DIRECTION ( 'NONE',  ( 0.000000000000000000, -1.000000000000000000, 0.000000000000000000 ) ) ;
#6001 = EDGE_LOOP ( 'NONE', ( #3434, #852 ) ) ;
#6002 =( NAMED_UNIT ( * ) PLANE_ANGLE_UNIT ( ) SI_UNIT ( $, .RADIAN. ) );
#6003 = CARTESIAN_POINT ( 'NONE',  ( -2.624999999999996891, -27.45833333333333570, 4.546633369868304797 ) ) ;
#6004 = EDGE_LOOP ( 'NONE', ( #6955, #7441, #5297, #5267, #7595, #5375, #883, #6048 ) ) ;
#6005 = CARTESIAN_POINT ( 'NONE',  ( 3.616337804771879580E-16, -29.54687500034139802, -5.905927827173866440 ) ) ;
#6006 = CARTESIAN_POINT ( 'NONE',  ( 2.134148098076978251, -4.449340926099361937, -2.108492589042307408 ) ) ;
#6007 = FACE_OUTER_BOUND ( 'NONE', #4922, .T. ) ;
#6008 = CARTESIAN_POINT ( 'NONE',  ( 0.000000000000000000, 79.00000000000001421, 0.000000000000000000 ) ) ;
#6009 = CARTESIAN_POINT ( 'NONE',  ( 2.557341765624996821, -28.21354166700806587, 4.429445870380401828 ) ) ;
#6010 = DIRECTION ( 'NONE',  ( 0.000000000000000000, 0.000000000000000000, -1.000000000000000000 ) ) ;
#6011 = CARTESIAN_POINT ( 'NONE',  ( -1.984762707500143719, -4.474939649318853872E-16, 2.802807230515030668 ) ) ;
#6012 = CARTESIAN_POINT ( 'NONE',  ( -5.114683531250000748, -27.73437500034139802, -6.263680815196995234E-16 ) ) ;
#6013 = EDGE_CURVE ( 'NONE', #1550, #3111, #2239, .T. ) ;
#6014 = VERTEX_POINT ( 'NONE', #6354 ) ;
#6015 = CARTESIAN_POINT ( 'NONE',  ( 7.041719095097280880E-16, -9.000000000000000000, -5.750000000000000000 ) ) ;
#6016 = CARTESIAN_POINT ( 'NONE',  ( 2.692658234374998738, -28.44270833299193413, -4.663820869356206877 ) ) ;
#6017 = EDGE_CURVE ( 'NONE', #4194, #1434, #2132, .T. ) ;
#6018 = CARTESIAN_POINT ( 'NONE',  ( 5.249999999999999112, -29.97916666666666430, -3.031088913245534755 ) ) ;
#6019 = CARTESIAN_POINT ( 'NONE',  ( -5.385316468749998364, -29.08854166632526628, 3.109213912904140287 ) ) ;
#6020 = ORIENTED_EDGE ( 'NONE', *, *, #7988, .F. ) ;
#6021 = CARTESIAN_POINT ( 'NONE',  ( 2.624999999999998668, -28.33333333333333215, -4.546633369868303021 ) ) ;
#6022 = CARTESIAN_POINT ( 'NONE',  ( -1.113604000661152470E-15, -27.59375000068279959, 6.062177826491070398 ) ) ;
#6023 = CARTESIAN_POINT ( 'NONE',  ( 5.385316468749999252, -28.21354166632526983, -3.109213912904139399 ) ) ;
#6024 = ORIENTED_EDGE ( 'NONE', *, *, #391, .T. ) ;
#6025 = CARTESIAN_POINT ( 'NONE',  ( -5.385316468749998364, -28.30729166632526628, 3.109213912904140287 ) ) ;
#6026 = CARTESIAN_POINT ( 'NONE',  ( 2.134148098076933397, -6.750659073900640017, 2.108492589042352261 ) ) ;
#6027 = DIRECTION ( 'NONE',  ( 0.000000000000000000, -1.000000000000000000, 0.000000000000000000 ) ) ;
#6028 = CARTESIAN_POINT ( 'NONE',  ( 6.429395695523604153E-16, -30.00000000000000000, -5.250000000000000000 ) ) ;
#6029 = CARTESIAN_POINT ( 'NONE',  ( -2.487701488670255312, -3.649340926099361226, 2.462045979635577808 ) ) ;
#6030 =( BOUNDED_CURVE ( )  B_SPLINE_CURVE ( 2, ( #3976, #5453, #480, #6106, #6805, #429, #1837, #3371, #8299 ),
 .UNSPECIFIED., .F., .F. ) 
 B_SPLINE_CURVE_WITH_KNOTS ( ( 3, 2, 2, 2, 3 ),
 ( 0.6458333333333333703, 0.6527777777777777901, 0.6666666666666666297, 0.6805555555555555802, 0.6875000000000000000 ),
 .UNSPECIFIED. ) 
 CURVE ( )  GEOMETRIC_REPRESENTATION_ITEM ( )  RATIONAL_B_SPLINE_CURVE ( ( 0.9330127018922192983, 0.9330127018922198534, 1.000000000000000000, 0.8660254037844387076, 1.000000000000000000, 0.8660254037844387076, 1.000000000000000000, 0.9330127018922194093, 0.9330127018922194093 ) ) 
 REPRESENTATION_ITEM ( '' )  );
#6031 = CARTESIAN_POINT ( 'NONE',  ( -1.084901341431563923E-15, -29.42187500034139447, 5.905927827173866440 ) ) ;
#6032 = EDGE_LOOP ( 'NONE', ( #8803, #5990, #2899, #5690 ) ) ;
#6033 = APPLICATION_PROTOCOL_DEFINITION ( 'draft international standard', 'automotive_design', 1998, #9134 ) ;
#6034 = CARTESIAN_POINT ( 'NONE',  ( -2.692658234375000514, -29.11979166632526983, -4.663820869356205989 ) ) ;
#6035 = CARTESIAN_POINT ( 'NONE',  ( -3.992485675378532939, -4.949340926099361937, -1.674995433905601683 ) ) ;
#6036 = FACE_OUTER_BOUND ( 'NONE', #519, .T. ) ;
#6037 = VERTEX_POINT ( 'NONE', #7716 ) ;
#6038 = CARTESIAN_POINT ( 'NONE',  ( 5.385316468749999252, -28.43229166632526983, -3.109213912904139399 ) ) ;
#6039 = CARTESIAN_POINT ( 'NONE',  ( -3.507514324621434199, -2.850659073900639662, -1.431606283892695064 ) ) ;
#6040 = ORIENTED_EDGE ( 'NONE', *, *, #1335, .F. ) ;
#6041 = CARTESIAN_POINT ( 'NONE',  ( -2.624999999999998668, -27.66666666666666430, -4.546633369868303021 ) ) ;
#6042 = CARTESIAN_POINT ( 'NONE',  ( -2.462045979635629323, -6.350659073900638774, 2.487701488670203798 ) ) ;
#6043 = EDGE_CURVE ( 'NONE', #4503, #8948, #7035, .T. ) ;
#6044 = CARTESIAN_POINT ( 'NONE',  ( 0.01814118441313990887, -3.350659073900639218, 3.500000000000000000 ) ) ;
#6045 = PRESENTATION_LAYER_ASSIGNMENT (  '', '', ( #3826 ) ) ;
#6046 = ORIENTED_EDGE ( 'NONE', *, *, #1730, .T. ) ;
#6047 = CARTESIAN_POINT ( 'NONE',  ( 1.113604000661152470E-15, -27.18750000000000000, 6.062177826491070398 ) ) ;
#6048 = ORIENTED_EDGE ( 'NONE', *, *, #652, .F. ) ;
#6049 = CARTESIAN_POINT ( 'NONE',  ( 5.114683531250000748, -29.10937500034139802, 0.000000000000000000 ) ) ;
#6050 = CARTESIAN_POINT ( 'NONE',  ( -3.000000000000000444, -3.449340926099361493, -0.01814118441320822922 ) ) ;
#6051 = DIRECTION ( 'NONE',  ( 1.039441819132097611E-14, 0.07256473765270715637, -0.9973637043974449279 ) ) ;
#6052 = CARTESIAN_POINT ( 'NONE',  ( 3.673940397442059375E-16, -46.00000000000000000, 2.999999999999999556 ) ) ;
#6053 = CARTESIAN_POINT ( 'NONE',  ( -1.084901341431563923E-15, -28.98437500034139447, 5.905927827173866440 ) ) ;
#6054 =( GEOMETRIC_REPRESENTATION_CONTEXT ( 3 ) GLOBAL_UNCERTAINTY_ASSIGNED_CONTEXT ( ( #2456 ) ) GLOBAL_UNIT_ASSIGNED_CONTEXT ( ( #8517, #693, #7025 ) ) REPRESENTATION_CONTEXT ( 'NONE', 'WORKASPACE' ) );
#6055 = LINE ( 'NONE', #2017, #6727 ) ;
#6056 = EDGE_CURVE ( 'NONE', #738, #8882, #6431, .T. ) ;
#6057 = CARTESIAN_POINT ( 'NONE',  ( -1.406733260263382856, -27.95758545099817027, -5.250000000000006217 ) ) ;
#6058 = LINE ( 'NONE', #7604, #1049 ) ;
#6059 = EDGE_CURVE ( 'NONE', #5951, #1550, #5504, .T. ) ;
#6060 = ORIENTED_EDGE ( 'NONE', *, *, #222, .T. ) ;
#6061 = CARTESIAN_POINT ( 'NONE',  ( 3.061616997868383141E-16, 74.00000000000001421, -2.500000000000000000 ) ) ;
#6062 = CARTESIAN_POINT ( 'NONE',  ( -5.385316468750001029, -28.63020833299193413, -3.109213912904136734 ) ) ;
#6063 = CARTESIAN_POINT ( 'NONE',  ( 1.142306659890740623E-15, -30.04687499965859487, 6.218427825808274356 ) ) ;
#6064 = DIRECTION ( 'NONE',  ( 0.000000000000000000, 1.000000000000000000, 0.000000000000000000 ) ) ;
#6065 = CARTESIAN_POINT ( 'NONE',  ( -3.807688866302469071E-16, -29.67187499965860198, -6.218427825808274356 ) ) ;
#6066 = CARTESIAN_POINT ( 'NONE',  ( 4.000000000000000000, -4.249340926099360871, 0.01814118441321914063 ) ) ;
#6067 = ORIENTED_EDGE ( 'NONE', *, *, #4471, .F. ) ;
#6068 = CARTESIAN_POINT ( 'NONE',  ( 0.000000000000000000, 79.00000000000001421, 0.000000000000000000 ) ) ;
#6069 = CARTESIAN_POINT ( 'NONE',  ( 3.712013335537174572E-16, -28.21875000068279604, -6.062177826491070398 ) ) ;
#6070 = CARTESIAN_POINT ( 'NONE',  ( -2.692658234374996518, -29.56770833299193413, 4.663820869356208654 ) ) ;
#6071 = ORIENTED_EDGE ( 'NONE', *, *, #3106, .F. ) ;
#6072 = CARTESIAN_POINT ( 'NONE',  ( -5.385316468750000141, -28.32812499965860198, 0.000000000000000000 ) ) ;
#6073 = CARTESIAN_POINT ( 'NONE',  ( -1.260781871532431708, -5.850659073900641438, -2.992485675378564469 ) ) ;
#6074 = DIRECTION ( 'NONE',  ( 0.000000000000000000, -1.000000000000000000, 0.000000000000000000 ) ) ;
#6075 = FACE_BOUND ( 'NONE', #5903, .T. ) ;
#6076 = DIRECTION ( 'NONE',  ( -0.000000000000000000, -1.000000000000000000, -0.000000000000000000 ) ) ;
#6077 = CIRCLE ( 'NONE', #8015, 5.750000000000000000 ) ;
#6078 = CARTESIAN_POINT ( 'NONE',  ( 2.462045979635577364, -7.249340926099360871, 2.487701488670255312 ) ) ;
#6079 = CARTESIAN_POINT ( 'NONE',  ( 5.249999999999999112, -29.72916666666666430, -3.031088913245534755 ) ) ;
#6080 = CARTESIAN_POINT ( 'NONE',  ( 0.000000000000000000, 1.000000000000000000, 0.000000000000000000 ) ) ;
#6081 = AXIS2_PLACEMENT_3D ( 'NONE', #8175, #3384, #2689 ) ;
#6082 = APPLICATION_PROTOCOL_DEFINITION ( 'draft international standard', 'automotive_design', 1998, #1831 ) ;
#6083 = DIRECTION ( 'NONE',  ( 0.000000000000000000, 1.000000000000000000, 0.000000000000000000 ) ) ;
#6084 = ADVANCED_FACE ( 'NONE', ( #4995 ), #6400, .T. ) ;
#6085 = CARTESIAN_POINT ( 'NONE',  ( 1.467888652719048226, -6.149340926099360338, -3.492485675378536047 ) ) ;
#6086 = DIRECTION ( 'NONE',  ( -0.000000000000000000, -1.000000000000000000, -0.000000000000000000 ) ) ;
#6087 = AXIS2_PLACEMENT_3D ( 'NONE', #533, #6161, #3460 ) ;
#6088 = CLOSED_SHELL ( 'NONE', ( #131, #8881, #6622, #7934, #2782, #4275, #8600, #9033, #3163, #8563, #5016, #6084, #6475 ) ) ;
#6089 = CARTESIAN_POINT ( 'NONE',  ( 5.385316468749999252, -28.68229166632526983, -3.109213912904139399 ) ) ;
#6090 = CARTESIAN_POINT ( 'NONE',  ( -0.01814118441313947866, -2.550659073900638951, -3.500000000000000000 ) ) ;
#6091 = ORIENTED_EDGE ( 'NONE', *, *, #5756, .T. ) ;
#6092 = DIRECTION ( 'NONE',  ( 0.000000000000000000, 0.000000000000000000, 1.000000000000000000 ) ) ;
#6093 = AXIS2_PLACEMENT_3D ( 'NONE', #4878, #3191, #1889 ) ;
#6094 = FACE_OUTER_BOUND ( 'NONE', #1883, .T. ) ;
#6095 =( BOUNDED_CURVE ( )  B_SPLINE_CURVE ( 2, ( #1737, #4573, #8691, #5245, #5989, #2415, #3722, #7907, #3030 ),
 .UNSPECIFIED., .F., .F. ) 
 B_SPLINE_CURVE_WITH_KNOTS ( ( 3, 2, 2, 2, 3 ),
 ( 0.7708333333333333703, 0.7777777777777777901, 0.7916666666666666297, 0.8055555555555555802, 0.8125000000000000000 ),
 .UNSPECIFIED. ) 
 CURVE ( )  GEOMETRIC_REPRESENTATION_ITEM ( )  RATIONAL_B_SPLINE_CURVE ( ( 0.9330127018922192983, 0.9330127018922198534, 1.000000000000000000, 0.8660254037844387076, 1.000000000000000000, 0.8660254037844387076, 1.000000000000000000, 0.9330127018922194093, 0.9330127018922194093 ) ) 
 REPRESENTATION_ITEM ( '' )  );
#6096 = CARTESIAN_POINT ( 'NONE',  ( -0.01814118441313947866, -4.150659073900639484, -3.500000000000000000 ) ) ;
#6097 = ORIENTED_EDGE ( 'NONE', *, *, #851, .F. ) ;
#6098 =( NAMED_UNIT ( * ) PLANE_ANGLE_UNIT ( ) SI_UNIT ( $, .RADIAN. ) );
#6099 = CARTESIAN_POINT ( 'NONE',  ( -5.250000000000000000, -28.99999999999999645, 0.000000000000000000 ) ) ;
#6100 = AXIS2_PLACEMENT_3D ( 'NONE', #1878, #7541, #1168 ) ;
#6101 = VERTEX_POINT ( 'NONE', #2928 ) ;
#6102 = CARTESIAN_POINT ( 'NONE',  ( 2.557341765625000818, -29.56770833367473017, -4.429445870380400052 ) ) ;
#6103 = CARTESIAN_POINT ( 'NONE',  ( 1.224499502706077214, -3.949340926099361493, 3.007514324621463508 ) ) ;
#6104 = CYLINDRICAL_SURFACE ( 'NONE', #8805, 6.250000000000000000 ) ;
#6105 = CARTESIAN_POINT ( 'NONE',  ( 5.114683531249998971, -28.69270833367473017, 2.952963913586936329 ) ) ;
#6106 = CARTESIAN_POINT ( 'NONE',  ( -5.249999999999997335, -29.16666666598386826, 3.031088913245538308 ) ) ;
#6107 = ADVANCED_FACE ( 'NONE', ( #1710 ), #8083, .T. ) ;
#6108 = CARTESIAN_POINT ( 'NONE',  ( 5.250000000000000000, -29.25000000000000000, 0.000000000000000000 ) ) ;
#6109 = CIRCLE ( 'NONE', #5360, 4.250000000000000000 ) ;
#6110 = DIRECTION ( 'NONE',  ( 0.000000000000000000, 1.000000000000000000, 0.000000000000000000 ) ) ;
#6111 = DIRECTION ( 'NONE',  ( 0.000000000000000000, 1.000000000000000000, 0.000000000000000000 ) ) ;
#6112 = CARTESIAN_POINT ( 'NONE',  ( -5.114683531250000748, -28.52604166700806587, 2.952963913586931888 ) ) ;
#6113 = EDGE_CURVE ( 'NONE', #4963, #4350, #5396, .T. ) ;
#6114 = VERTEX_POINT ( 'NONE', #261 ) ;
#6115 = CARTESIAN_POINT ( 'NONE',  ( 5.385316468749999252, -28.96354166632526983, -3.109213912904138954 ) ) ;
#6116 = CARTESIAN_POINT ( 'NONE',  ( -1.406733260263393293, -29.20758545099816317, -5.250000000000000000 ) ) ;
#6117 = CARTESIAN_POINT ( 'NONE',  ( -5.385316468749998364, -28.83854166632526628, 3.109213912904140287 ) ) ;
#6118 = CARTESIAN_POINT ( 'NONE',  ( -2.815599370228846876, -8.049340926099359805, -2.841254879263533262 ) ) ;
#6119 = ORIENTED_EDGE ( 'NONE', *, *, #5422, .T. ) ;
#6120 = EDGE_CURVE ( 'NONE', #179, #1166, #2286, .T. ) ;
#6121 = CARTESIAN_POINT ( 'NONE',  ( 0.000000000000000000, 70.00000000000000000, 0.000000000000000000 ) ) ;
#6122 = CARTESIAN_POINT ( 'NONE',  ( -2.624999999999998668, -27.69791666734946389, -4.546633369868303021 ) ) ;
#6123 = CARTESIAN_POINT ( 'NONE',  ( 5.385316468749999252, -28.71354166632526628, -3.109213912904139399 ) ) ;
#6124 = ORIENTED_EDGE ( 'NONE', *, *, #8283, .F. ) ;
#6125 = CARTESIAN_POINT ( 'NONE',  ( 5.385316468749999252, -28.18229166632526628, -3.109213912904138954 ) ) ;
#6126 = CARTESIAN_POINT ( 'NONE',  ( 2.462045979635629767, -2.350659073900639218, -2.487701488670203354 ) ) ;
#6127 = FACE_OUTER_BOUND ( 'NONE', #4418, .T. ) ;
#6128 = ADVANCED_FACE ( 'NONE', ( #218 ), #124, .T. ) ;
#6129 = CARTESIAN_POINT ( 'NONE',  ( -1.406733260263390628, -28.82366454968462577, 5.250000000000001776 ) ) ;
#6130 = CYLINDRICAL_SURFACE ( 'NONE', #3766, 5.250000000000000000 ) ;
#6131 = CARTESIAN_POINT ( 'NONE',  ( 1.467888652719048226, -7.749340926099361759, -3.492485675378535603 ) ) ;
#6132 = AXIS2_PLACEMENT_3D ( 'NONE', #1894, #9085, #5552 ) ;
#6133 = CARTESIAN_POINT ( 'NONE',  ( 3.616337804771879580E-16, -29.29687500034139447, -5.905927827173866440 ) ) ;
#6134 = FACE_OUTER_BOUND ( 'NONE', #1457, .T. ) ;
#6135 = SHAPE_DEFINITION_REPRESENTATION ( #4262, #735 ) ;
#6136 = CARTESIAN_POINT ( 'NONE',  ( -2.692658234375000514, -28.86979166632526983, -4.663820869356205989 ) ) ;
#6137 = EDGE_CURVE ( 'NONE', #8090, #1056, #794, .T. ) ;
#6138 = CARTESIAN_POINT ( 'NONE',  ( 1.431606283892619125, -7.149340926099362115, 3.507514324621464397 ) ) ;
#6139 = CYLINDRICAL_SURFACE ( 'NONE', #6819, 2.999999999999999556 ) ;
#6140 = AXIS2_PLACEMENT_3D ( 'NONE', #3396, #3210, #1998 ) ;
#6141 = CARTESIAN_POINT ( 'NONE',  ( 1.142306659890740623E-15, -29.01562499965860198, 6.218427825808274356 ) ) ;
#6142 = EDGE_CURVE ( 'NONE', #3963, #8099, #4146, .T. ) ;
#6143 = CARTESIAN_POINT ( 'NONE',  ( 3.492485675378566690, -2.250659073900639573, -1.467888652718972287 ) ) ;
#6144 = ORIENTED_EDGE ( 'NONE', *, *, #8067, .F. ) ;
#6145 = CARTESIAN_POINT ( 'NONE',  ( -2.625000000000002220, -27.11458333401612819, 4.546633369868302132 ) ) ;
#6146 = DIRECTION ( 'NONE',  ( 0.000000000000000000, 0.000000000000000000, 1.000000000000000000 ) ) ;
#6147 = CARTESIAN_POINT ( 'NONE',  ( 5.114683531249998971, -27.19270833367473017, 2.952963913586936329 ) ) ;
#6148 = VECTOR ( 'NONE', #2125, 1000.000000000000000 ) ;
#6149 = ORIENTED_EDGE ( 'NONE', *, *, #2638, .F. ) ;
#6150 = PRESENTATION_STYLE_ASSIGNMENT (( #7545 ) ) ;
#6151 = CARTESIAN_POINT ( 'NONE',  ( -2.624999999999996891, -27.95833333333333215, 4.546633369868304797 ) ) ;
#6152 = ORIENTED_EDGE ( 'NONE', *, *, #1197, .F. ) ;
#6153 = CARTESIAN_POINT ( 'NONE',  ( 2.557341765624996821, -28.65104166700806587, 4.429445870380401828 ) ) ;
#6154 = CARTESIAN_POINT ( 'NONE',  ( 1.224499502706077214, -2.349340926099361848, 3.007514324621463508 ) ) ;
#6155 = DIRECTION ( 'NONE',  ( 0.000000000000000000, 0.000000000000000000, 1.000000000000000000 ) ) ;
#6156 = CARTESIAN_POINT ( 'NONE',  ( 2.557341765624996821, -27.71354166700806587, 4.429445870380401828 ) ) ;
#6157 = CARTESIAN_POINT ( 'NONE',  ( 0.000000000000000000, -20.00000000000000000, 0.000000000000000000 ) ) ;
#6158 =( BOUNDED_CURVE ( )  B_SPLINE_CURVE ( 2, ( #3840, #8672, #2919, #809, #3652, #6477, #7974, #2961, #112 ),
 .UNSPECIFIED., .F., .F. ) 
 B_SPLINE_CURVE_WITH_KNOTS ( ( 3, 2, 2, 2, 3 ),
 ( 0.8541666666666667407, 0.8611111111111111605, 0.8750000000000000000, 0.8888888888888888395, 0.8958333333333333703 ),
 .UNSPECIFIED. ) 
 CURVE ( )  GEOMETRIC_REPRESENTATION_ITEM ( )  RATIONAL_B_SPLINE_CURVE ( ( 0.9330127018922192983, 0.9330127018922198534, 1.000000000000000000, 0.8660254037844387076, 1.000000000000000000, 0.8660254037844387076, 1.000000000000000000, 0.9330127018922187432, 0.9330127018922192983 ) ) 
 REPRESENTATION_ITEM ( '' )  );
#6159 = LINE ( 'NONE', #9115, #3721 ) ;
#6160 = CARTESIAN_POINT ( 'NONE',  ( 5.114683531250000748, -29.92187500034139802, 0.000000000000000000 ) ) ;
#6161 = DIRECTION ( 'NONE',  ( -0.000000000000000000, -1.000000000000000000, -0.000000000000000000 ) ) ;
#6162 = CARTESIAN_POINT ( 'NONE',  ( 5.114683531249999859, -29.65104166700806232, -2.952963913586932776 ) ) ;
#6163 = CARTESIAN_POINT ( 'NONE',  ( 0.000000000000000000, 73.00000000000001421, 0.000000000000000000 ) ) ;
#6164 = CARTESIAN_POINT ( 'NONE',  ( 5.385316468750001029, -28.75520833299193413, 3.109213912904134958 ) ) ;
#6165 = PLANE ( 'NONE',  #6569 ) ;
#6166 = FACE_OUTER_BOUND ( 'NONE', #4391, .T. ) ;
#6167 = CARTESIAN_POINT ( 'NONE',  ( -2.692658234375000514, -29.15104166632526983, -4.663820869356205989 ) ) ;
#6168 = CARTESIAN_POINT ( 'NONE',  ( 3.507514324621465285, -4.349340926099361404, -1.431606283892619125 ) ) ;
#6169 = CARTESIAN_POINT ( 'NONE',  ( -0.01814118441321889430, -7.049340926099361582, 4.000000000000000000 ) ) ;
#6170 = ORIENTED_EDGE ( 'NONE', *, *, #1794, .T. ) ;
#6171 = CYLINDRICAL_SURFACE ( 'NONE', #6081, 5.250000000000000000 ) ;
#6172 = CARTESIAN_POINT ( 'NONE',  ( 5.249999999999999112, -28.30208333401612819, 3.031088913245538308 ) ) ;
#6173 = CARTESIAN_POINT ( 'NONE',  ( 5.385316468750001029, -29.25520833299193058, 3.109213912904135846 ) ) ;
#6174 = ADVANCED_FACE ( 'NONE', ( #3160, #5980 ), #3663, .T. ) ;
#6175 = VERTEX_POINT ( 'NONE', #5095 ) ;
#6176 = CARTESIAN_POINT ( 'NONE',  ( -5.385316468750001029, -28.59895833299193413, -3.109213912904136734 ) ) ;
#6177 = CARTESIAN_POINT ( 'NONE',  ( -1.431606283892693066, -0.05065907390063895815, 3.507514324621434199 ) ) ;
#6178 = CARTESIAN_POINT ( 'NONE',  ( 5.249999999999997335, -29.52083333333333215, 3.031088913245538308 ) ) ;
#6179 =( BOUNDED_CURVE ( )  B_SPLINE_CURVE ( 2, ( #4850, #2819, #7696, #5596, #1321 ),
 .UNSPECIFIED., .F., .T. ) 
 B_SPLINE_CURVE_WITH_KNOTS ( ( 3, 2, 3 ),
 ( 0.000000000000000000, 0.01388888888888888985, 0.02083333333333333565 ),
 .UNSPECIFIED. ) 
 CURVE ( )  GEOMETRIC_REPRESENTATION_ITEM ( )  RATIONAL_B_SPLINE_CURVE ( ( 1.000000000000000000, 0.8660254037844387076, 1.000000000000000000, 0.9330127018922192983, 0.9330127018922194093 ) ) 
 REPRESENTATION_ITEM ( '' )  );
#6180 = DIRECTION ( 'NONE',  ( 1.000000000000000000, 0.000000000000000000, 0.000000000000000000 ) ) ;
#6181 = FACE_OUTER_BOUND ( 'NONE', #6917, .T. ) ;
#6182 = CARTESIAN_POINT ( 'NONE',  ( 2.487701488670255756, -7.649340926099361226, -2.462045979635577364 ) ) ;
#6183 = DIRECTION ( 'NONE',  ( 0.000000000000000000, 0.000000000000000000, -1.000000000000000000 ) ) ;
#6184 = DIRECTION ( 'NONE',  ( 0.000000000000000000, -1.000000000000000000, 0.000000000000000000 ) ) ;
#6185 = SHAPE_DEFINITION_REPRESENTATION ( #99, #1843 ) ;
#6186 = CARTESIAN_POINT ( 'NONE',  ( 2.692658234374998738, -29.41145833299193413, -4.663820869356206877 ) ) ;
#6187 = CARTESIAN_POINT ( 'NONE',  ( -0.01814118441321365544, -7.049340926099361582, 3.500000000000000000 ) ) ;
#6188 = CARTESIAN_POINT ( 'NONE',  ( 1.975475456537005874E-15, -27.93749999999999289, 5.250000000000000000 ) ) ;
#6189 = CARTESIAN_POINT ( 'NONE',  ( -5.385316468750001029, -29.59895833299193413, -3.109213912904136734 ) ) ;
#6190 = CARTESIAN_POINT ( 'NONE',  ( -3.492485675378566246, -1.450659073900639084, 1.467888652718973397 ) ) ;
#6191 = ORIENTED_EDGE ( 'NONE', *, *, #2736, .T. ) ;
#6192 = CARTESIAN_POINT ( 'NONE',  ( -1.113604000661152470E-15, -27.06250000000000000, 6.062177826491070398 ) ) ;
#6193 = CARTESIAN_POINT ( 'NONE',  ( 1.000000000000000000, -35.00000000000000000, 2.880243826144208708 ) ) ;
#6194 = CARTESIAN_POINT ( 'NONE',  ( 2.487701488670203354, -5.150659073900639484, 2.462045979635629323 ) ) ;
#6195 = ORIENTED_EDGE ( 'NONE', *, *, #5013, .F. ) ;
#6196 = SURFACE_SIDE_STYLE ('',( #8291 ) ) ;
#6197 = CARTESIAN_POINT ( 'NONE',  ( 2.624999999999998668, -28.08333333333333215, -4.546633369868303021 ) ) ;
#6198 = CARTESIAN_POINT ( 'NONE',  ( 3.616337804771879580E-16, -27.29687500034139802, -5.905927827173866440 ) ) ;
#6199 = CARTESIAN_POINT ( 'NONE',  ( 1.431606283892619125, -7.149340926099362115, 3.507514324621464397 ) ) ;
#6200 = DIRECTION ( 'NONE',  ( 0.000000000000000000, 0.000000000000000000, 1.000000000000000000 ) ) ;
#6201 = CARTESIAN_POINT ( 'NONE',  ( 5.114683531249999859, -27.40104166700806587, -2.952963913586932776 ) ) ;
#6202 = CARTESIAN_POINT ( 'NONE',  ( 1.406733260263405061, -27.22991455036742536, -5.249999999999994671 ) ) ;
#6203 = CARTESIAN_POINT ( 'NONE',  ( 5.114683531250000748, -29.17187500034139802, 0.000000000000000000 ) ) ;
#6204 = CARTESIAN_POINT ( 'NONE',  ( -5.249999999999999112, -28.39583333333333215, -3.031088913245536975 ) ) ;
#6205 = CARTESIAN_POINT ( 'NONE',  ( -1.084901341431563923E-15, -29.48437500034139802, 5.905927827173866440 ) ) ;
#6206 = AXIS2_PLACEMENT_3D ( 'NONE', #5947, #6733, #8646 ) ;
#6207 = CARTESIAN_POINT ( 'NONE',  ( -2.033577675846918216E-14, -29.18750000000000355, 5.250000000000000888 ) ) ;
#6208 = EDGE_CURVE ( 'NONE', #3979, #2331, #2902, .T. ) ;
#6209 = CARTESIAN_POINT ( 'NONE',  ( 5.250000000000000000, -29.04166666598387181, -3.031088913245536531 ) ) ;
#6210 = CARTESIAN_POINT ( 'NONE',  ( -2.692658234374996518, -29.81770833299193413, 4.663820869356208654 ) ) ;
#6211 = CARTESIAN_POINT ( 'NONE',  ( 0.000000000000000000, -28.00000000000000000, -2.750000000000000000 ) ) ;
#6212 = CARTESIAN_POINT ( 'NONE',  ( -5.385316468749998364, -29.33854166632526983, 3.109213912904140287 ) ) ;
#6213 = CARTESIAN_POINT ( 'NONE',  ( 1.431606283892619125, -2.349340926099361848, 3.507514324621464397 ) ) ;
#6214 = CARTESIAN_POINT ( 'NONE',  ( -0.01814118441321889430, -5.449340926099361937, 4.000000000000000000 ) ) ;
#6215 = ORIENTED_EDGE ( 'NONE', *, *, #8454, .F. ) ;
#6216 = CARTESIAN_POINT ( 'NONE',  ( 0.000000000000000000, 81.00000000000001421, 0.000000000000000000 ) ) ;
#6217 = CARTESIAN_POINT ( 'NONE',  ( 5.250000000000000000, -27.76041666734946389, -3.031088913245534755 ) ) ;
#6218 = CARTESIAN_POINT ( 'NONE',  ( -5.385316468750000141, -29.10937499965859843, 0.000000000000000000 ) ) ;
#6219 = ORIENTED_EDGE ( 'NONE', *, *, #6789, .F. ) ;
#6220 = CARTESIAN_POINT ( 'NONE',  ( 2.692658234374998738, -27.91145833299193413, -4.663820869356206877 ) ) ;
#6221 = CARTESIAN_POINT ( 'NONE',  ( -2.134148098076932953, -7.550659073900640728, -2.108492589042352705 ) ) ;
#6222 = DIRECTION ( 'NONE',  ( -0.000000000000000000, 1.000000000000000000, -0.000000000000000000 ) ) ;
#6223 = CARTESIAN_POINT ( 'NONE',  ( -9.180150650966086169E-15, -28.43750000000000000, 5.249999999999999112 ) ) ;
#6224 = CARTESIAN_POINT ( 'NONE',  ( 0.000000000000000000, -27.00000000000000000, 0.000000000000000000 ) ) ;
#6225 = CARTESIAN_POINT ( 'NONE',  ( -1.431606283892620235, -7.949340926099361049, -3.507514324621463953 ) ) ;
#6226 =( REPRESENTATION_RELATIONSHIP ('NONE','NONE', #735, #2791 ) REPRESENTATION_RELATIONSHIP_WITH_TRANSFORMATION ( #6399 )SHAPE_REPRESENTATION_RELATIONSHIP( ) );
#6227 = CARTESIAN_POINT ( 'NONE',  ( 2.557341765625000818, -29.06770833367473017, -4.429445870380400052 ) ) ;
#6228 = CARTESIAN_POINT ( 'NONE',  ( 5.249999999999997335, -27.55208333401612819, 3.031088913245538308 ) ) ;
#6229 = PRODUCT_CONTEXT ( 'NONE', #2753, 'mechanical' ) ;
#6230 = CARTESIAN_POINT ( 'NONE',  ( 2.692658234374998738, -29.16145833299193413, -4.663820869356206877 ) ) ;
#6231 = CARTESIAN_POINT ( 'NONE',  ( -1.467888652719046449, -5.349340926099361404, 3.492485675378536047 ) ) ;
#6232 = CARTESIAN_POINT ( 'NONE',  ( 5.250000000000000000, -27.00000000000000000, 0.000000000000000000 ) ) ;
#6233 =( BOUNDED_CURVE ( )  B_SPLINE_CURVE ( 2, ( #8183, #8370, #8962, #4047, #6879, #2611, #360, #8275, #1908 ),
 .UNSPECIFIED., .F., .F. ) 
 B_SPLINE_CURVE_WITH_KNOTS ( ( 3, 2, 2, 2, 3 ),
 ( 0.3958333333333333703, 0.4027777777777777901, 0.4166666666666666852, 0.4305555555555555802, 0.4375000000000000000 ),
 .UNSPECIFIED. ) 
 CURVE ( )  GEOMETRIC_REPRESENTATION_ITEM ( )  RATIONAL_B_SPLINE_CURVE ( ( 0.9330127018922194093, 0.9330127018922196314, 1.000000000000000000, 0.8660254037844387076, 1.000000000000000000, 0.8660254037844387076, 1.000000000000000000, 0.9330127018922194093, 0.9330127018922194093 ) ) 
 REPRESENTATION_ITEM ( '' )  );
#6234 = CARTESIAN_POINT ( 'NONE',  ( 5.385316468749999252, -29.43229166632526983, -3.109213912904139399 ) ) ;
#6235 = CARTESIAN_POINT ( 'NONE',  ( 1.674995433905515085, -3.450659073900638862, 3.992485675378568022 ) ) ;
#6236 = CARTESIAN_POINT ( 'NONE',  ( -2.624999999999998668, -27.16666666666666430, -4.546633369868303021 ) ) ;
#6237 = LINE ( 'NONE', #4058, #8336 ) ;
#6238 = ADVANCED_FACE ( 'NONE', ( #7050 ), #2165, .F. ) ;
#6239 = EDGE_LOOP ( 'NONE', ( #158, #235, #7390, #7476 ) ) ;
#6240 = CARTESIAN_POINT ( 'NONE',  ( 5.250000000000000888, -27.89583333333332860, 3.031088913245532979 ) ) ;
#6241 = CARTESIAN_POINT ( 'NONE',  ( 5.114683531250000748, -27.60937500034139802, 0.000000000000000000 ) ) ;
#6242 = CARTESIAN_POINT ( 'NONE',  ( 2.108492589042352705, -0.7506590739006395729, -2.134148098076933397 ) ) ;
#6243 = DIRECTION ( 'NONE',  ( 0.000000000000000000, -1.000000000000000000, 0.000000000000000000 ) ) ;
#6244 = AXIS2_PLACEMENT_3D ( 'NONE', #8057, #5820, #4476 ) ;
#6245 = CARTESIAN_POINT ( 'NONE',  ( -5.250000000000000000, -29.87500000000000000, -6.429395695523604153E-16 ) ) ;
#6246 = CARTESIAN_POINT ( 'NONE',  ( 8.603239422292021091E-08, -29.99999999999999645, -5.249999999999998224 ) ) ;
#6247 = AXIS2_PLACEMENT_3D ( 'NONE', #8278, #4692, #3863 ) ;
#6248 = CARTESIAN_POINT ( 'NONE',  ( 5.114683531250000748, -28.65104166700806587, -2.952963913586932776 ) ) ;
#6249 = CIRCLE ( 'NONE', #4905, 2.000000000000000000 ) ;
#6250 = CARTESIAN_POINT ( 'NONE',  ( -2.557341765625002594, -29.25520833367473017, 4.429445870380399164 ) ) ;
#6251 = CARTESIAN_POINT ( 'NONE',  ( -2.033577675846918216E-14, -29.68750000000000355, 5.250000000000000888 ) ) ;
#6252 = CARTESIAN_POINT ( 'NONE',  ( 5.250000000000000888, -29.33333333265053255, 3.031088913245532979 ) ) ;
#6253 = CARTESIAN_POINT ( 'NONE',  ( -5.385316468750000141, -30.10937499965859843, 0.000000000000000000 ) ) ;
#6254 = CARTESIAN_POINT ( 'NONE',  ( 2.625000000000000444, -29.48958333401613174, -4.546633369868303021 ) ) ;
#6255 = DIRECTION ( 'NONE',  ( 0.000000000000000000, -1.000000000000000000, 0.000000000000000000 ) ) ;
#6256 = CARTESIAN_POINT ( 'NONE',  ( 3.500000000000000000, -1.049340926099360916, 0.01814118441321387054 ) ) ;
#6257 = CARTESIAN_POINT ( 'NONE',  ( -4.000000000000000000, -6.649340926099362115, -0.01814118441321865144 ) ) ;
#6258 = VERTEX_POINT ( 'NONE', #2694 ) ;
#6259 = PRESENTATION_LAYER_ASSIGNMENT (  '', '', ( #8174 ) ) ;
#6260 = CARTESIAN_POINT ( 'NONE',  ( -2.033577675846918216E-14, -29.18750000000000355, 5.250000000000000888 ) ) ;
#6261 = CARTESIAN_POINT ( 'NONE',  ( -5.114683531250000748, -29.46354166700806232, 2.952963913586931888 ) ) ;
#6262 = CARTESIAN_POINT ( 'NONE',  ( -5.250000000000000000, -27.20833333265053966, -3.031088913245534755 ) ) ;
#6263 = VERTEX_POINT ( 'NONE', #6388 ) ;
#6264 = CARTESIAN_POINT ( 'NONE',  ( -5.385316468750000141, -29.32812499965859843, 0.000000000000000000 ) ) ;
#6265 = CARTESIAN_POINT ( 'NONE',  ( 2.841254879263473310, -1.950659073900638640, 2.815599370228907272 ) ) ;
#6266 = CARTESIAN_POINT ( 'NONE',  ( 1.000000000000000000, -35.00000000000000000, -3.048902179152658931 ) ) ;
#6267 = DIRECTION ( 'NONE',  ( 0.000000000000000000, -1.000000000000000000, 0.000000000000000000 ) ) ;
#6268 = CARTESIAN_POINT ( 'NONE',  ( 0.000000000000000000, -27.00000000000000000, -5.250000000000000000 ) ) ;
#6269 = CARTESIAN_POINT ( 'NONE',  ( 5.114683531250000748, -28.60937500034139802, 0.000000000000000000 ) ) ;
#6270 = CARTESIAN_POINT ( 'NONE',  ( 5.250000000000000888, -28.33333333265052900, 3.031088913245533423 ) ) ;
#6271 = CARTESIAN_POINT ( 'NONE',  ( 2.625000000000002220, -27.85416666598386826, 4.546633369868302132 ) ) ;
#6272 = CARTESIAN_POINT ( 'NONE',  ( -2.134148098076978251, -0.4493409260993615484, 2.108492589042307408 ) ) ;
#6273 = CARTESIAN_POINT ( 'NONE',  ( -1.406733260263389518, -28.05133545031536357, -5.250000000000001776 ) ) ;
#6274 = CARTESIAN_POINT ( 'NONE',  ( -5.385316468750000141, -29.57812499965859843, 0.000000000000000000 ) ) ;
#6275 = EDGE_CURVE ( 'NONE', #4568, #1724, #5994, .T. ) ;
#6276 = CARTESIAN_POINT ( 'NONE',  ( -3.992485675378568022, -3.050659073900638951, 1.674995433905515529 ) ) ;
#6277 = DIRECTION ( 'NONE',  ( 0.000000000000000000, 1.000000000000000000, 0.000000000000000000 ) ) ;
#6278 = CARTESIAN_POINT ( 'NONE',  ( 9.180150650966086169E-15, -28.59375000068279959, 5.250000000000000000 ) ) ;
#6279 = EDGE_CURVE ( 'NONE', #116, #7863, #3931, .T. ) ;
#6280 = ORIENTED_EDGE ( 'NONE', *, *, #3787, .F. ) ;
#6281 = CARTESIAN_POINT ( 'NONE',  ( -2.624999999999996891, -28.20833333333333215, 4.546633369868304797 ) ) ;
#6282 = AXIS2_PLACEMENT_3D ( 'NONE', #6514, #151, #3001 ) ;
#6283 = CARTESIAN_POINT ( 'NONE',  ( 5.114683531249998971, -27.88020833367473017, 2.952963913586936329 ) ) ;
#6284 = CARTESIAN_POINT ( 'NONE',  ( 1.224499502706142273, -2.450659073900639751, -3.007514324621435531 ) ) ;
#6285 = CARTESIAN_POINT ( 'NONE',  ( 2.557341765624996821, -26.96354166700806232, 4.429445870380401828 ) ) ;
#6286 = FACE_OUTER_BOUND ( 'NONE', #6701, .T. ) ;
#6287 = AXIS2_PLACEMENT_3D ( 'NONE', #2050, #606, #8335 ) ;
#6288 = PRESENTATION_LAYER_ASSIGNMENT (  '', '', ( #8813 ) ) ;
#6289 = CARTESIAN_POINT ( 'NONE',  ( -2.557341765624999042, -28.83854166700806587, -4.429445870380400052 ) ) ;
#6290 = CARTESIAN_POINT ( 'NONE',  ( -2.557341765625002594, -28.50520833367473017, 4.429445870380399164 ) ) ;
#6291 = CARTESIAN_POINT ( 'NONE',  ( -1.406733260263391960, -28.69866454968462577, 5.250000000000000000 ) ) ;
#6292 = CARTESIAN_POINT ( 'NONE',  ( 1.113604000661152470E-15, -29.62499999931720041, 6.062177826491070398 ) ) ;
#6293 = DIRECTION ( 'NONE',  ( 0.000000000000000000, 0.000000000000000000, -1.000000000000000000 ) ) ;
#6294 = AXIS2_PLACEMENT_3D ( 'NONE', #328, #8704, #4475 ) ;
#6295 = CARTESIAN_POINT ( 'NONE',  ( 5.249999999999999112, -28.47916666666666785, -3.031088913245534755 ) ) ;
#6296 = CARTESIAN_POINT ( 'NONE',  ( 3.492485675378536047, -0.9493409260993610488, 1.467888652719046672 ) ) ;
#6297 = EDGE_LOOP ( 'NONE', ( #6732, #3896, #2806, #208 ) ) ;
#6298 = ADVANCED_BREP_SHAPE_REPRESENTATION ( '', ( #2148, #888 ), #5908 ) ;
#6299 = CARTESIAN_POINT ( 'NONE',  ( -2.624999999999996891, -29.64583333265053611, 4.546633369868304797 ) ) ;
#6300 = CARTESIAN_POINT ( 'NONE',  ( 2.625000000000000444, -26.98958333401612819, -4.546633369868303021 ) ) ;
#6301 = EDGE_CURVE ( 'NONE', #3979, #6553, #7277, .T. ) ;
#6302 = EDGE_LOOP ( 'NONE', ( #1853, #408 ) ) ;
#6303 = CARTESIAN_POINT ( 'NONE',  ( 5.385316468750001029, -29.72395833299193413, 3.109213912904134958 ) ) ;
#6304 = CARTESIAN_POINT ( 'NONE',  ( 3.492485675378566690, -7.050659073900641616, -1.467888652718972287 ) ) ;
#6305 = CARTESIAN_POINT ( 'NONE',  ( -1.406733260263385521, -27.07366454968463287, 5.250000000000006217 ) ) ;
#6306 = DIRECTION ( 'NONE',  ( 0.000000000000000000, 0.000000000000000000, -1.000000000000000000 ) ) ;
#6307 = DIRECTION ( 'NONE',  ( 0.000000000000000000, -1.000000000000000000, 0.000000000000000000 ) ) ;
#6308 = CARTESIAN_POINT ( 'NONE',  ( 5.249999999999999112, -28.85416666666667140, -3.031088913245536975 ) ) ;
#6309 = EDGE_CURVE ( 'NONE', #4663, #2713, #7492, .T. ) ;
#6310 = CARTESIAN_POINT ( 'NONE',  ( -2.557341765624999042, -29.02604166700806587, -4.429445870380400052 ) ) ;
#6311 = CARTESIAN_POINT ( 'NONE',  ( -1.925759277493323207, -9.035843541029837430E-14, 2.922632427747480222 ) ) ;
#6312 = CARTESIAN_POINT ( 'NONE',  ( -6.972266317189433020E-16, -27.74999999931720041, -5.250000000000000000 ) ) ;
#6313 = CARTESIAN_POINT ( 'NONE',  ( -1.260781871532494103, -6.949340926099362825, 2.992485675378538712 ) ) ;
#6314 = DIRECTION ( 'NONE',  ( 0.000000000000000000, 0.000000000000000000, -1.000000000000000000 ) ) ;
#6315 = CARTESIAN_POINT ( 'NONE',  ( 1.142306659890740623E-15, -30.01562499965860198, 6.218427825808274356 ) ) ;
#6316 = CARTESIAN_POINT ( 'NONE',  ( -4.000000000000000000, -2.950659073900638862, 0.01814118441313491634 ) ) ;
#6317 = CARTESIAN_POINT ( 'NONE',  ( -7.654042494670960565E-16, -30.00000000000000000, 6.250000000000002665 ) ) ;
#6318 = ORIENTED_EDGE ( 'NONE', *, *, #1165, .T. ) ;
#6319 =( NAMED_UNIT ( * ) SI_UNIT ( $, .STERADIAN. ) SOLID_ANGLE_UNIT ( ) );
#6320 = CARTESIAN_POINT ( 'NONE',  ( 1.113604000661152470E-15, -29.68750000000000000, 6.062177826491070398 ) ) ;
#6321 = EDGE_LOOP ( 'NONE', ( #3256, #9044, #5110, #1911 ) ) ;
#6322 = CARTESIAN_POINT ( 'NONE',  ( -2.557341765625002594, -27.94270833367473017, 4.429445870380399164 ) ) ;
#6323 = CARTESIAN_POINT ( 'NONE',  ( 2.134148098076933397, -0.3506590739006394397, 2.108492589042352261 ) ) ;
#6324 = CARTESIAN_POINT ( 'NONE',  ( 5.114683531249999859, -27.65104166700806232, -2.952963913586932776 ) ) ;
#6325 = FACE_OUTER_BOUND ( 'NONE', #2379, .T. ) ;
#6326 = EDGE_CURVE ( 'NONE', #566, #8116, #7369, .T. ) ;
#6327 = CARTESIAN_POINT ( 'NONE',  ( 2.557341765624996821, -28.71354166700806587, 4.429445870380401828 ) ) ;
#6328 = CARTESIAN_POINT ( 'NONE',  ( 0.000000000000000000, 0.000000000000000000, 0.000000000000000000 ) ) ;
#6329 = CARTESIAN_POINT ( 'NONE',  ( -1.084901341431563923E-15, -27.98437500034139802, 5.905927827173866440 ) ) ;
#6330 = CARTESIAN_POINT ( 'NONE',  ( -2.625000000000000444, -28.79166666666666785, -4.546633369868303021 ) ) ;
#6331 = CARTESIAN_POINT ( 'NONE',  ( -5.249999999999999112, -29.16666666598387181, 3.031088913245538308 ) ) ;
#6332 = LINE ( 'NONE', #2109, #2424 ) ;
#6333 = CARTESIAN_POINT ( 'NONE',  ( -1.942253529302216952, 2.864554167741711444E-18, 2.933213925443324488 ) ) ;
#6334 = CARTESIAN_POINT ( 'NONE',  ( -5.385316468750000141, -30.10937499965859843, 0.000000000000000000 ) ) ;
#6335 = CARTESIAN_POINT ( 'NONE',  ( 3.492485675378536047, -4.149340926099361226, 1.467888652719046672 ) ) ;
#6336 = CARTESIAN_POINT ( 'NONE',  ( -3.492485675378536047, -4.949340926099361049, -1.467888652719048670 ) ) ;
#6337 = EDGE_CURVE ( 'NONE', #6768, #6698, #6746, .T. ) ;
#6338 = ORIENTED_EDGE ( 'NONE', *, *, #97, .F. ) ;
#6339 = CARTESIAN_POINT ( 'NONE',  ( -1.406733260263391960, -29.63616454900182973, 5.250000000000000000 ) ) ;
#6340 = CARTESIAN_POINT ( 'NONE',  ( 2.557341765624996821, -29.40104166700806232, 4.429445870380401828 ) ) ;
#6341 = EDGE_CURVE ( 'NONE', #4820, #1374, #3846, .T. ) ;
#6342 =( GEOMETRIC_REPRESENTATION_CONTEXT ( 3 ) GLOBAL_UNCERTAINTY_ASSIGNED_CONTEXT ( ( #3763 ) ) GLOBAL_UNIT_ASSIGNED_CONTEXT ( ( #145, #7872, #3546 ) ) REPRESENTATION_CONTEXT ( 'NONE', 'WORKASPACE' ) );
#6343 = VERTEX_POINT ( 'NONE', #5127 ) ;
#6344 = CARTESIAN_POINT ( 'NONE',  ( -3.807688866302469071E-16, -29.64062499965859843, -6.218427825808274356 ) ) ;
#6345 = CARTESIAN_POINT ( 'NONE',  ( -2.815599370228907272, 0.04934092609936149149, 2.841254879263473754 ) ) ;
#6346 = CARTESIAN_POINT ( 'NONE',  ( -1.975475456537005874E-15, -28.09375000068279604, 5.249999999999999112 ) ) ;
#6347 = ORIENTED_EDGE ( 'NONE', *, *, #2711, .T. ) ;
#6348 =( GEOMETRIC_REPRESENTATION_CONTEXT ( 3 ) GLOBAL_UNCERTAINTY_ASSIGNED_CONTEXT ( ( #6534 ) ) GLOBAL_UNIT_ASSIGNED_CONTEXT ( ( #7068, #2804, #3538 ) ) REPRESENTATION_CONTEXT ( 'NONE', 'WORKASPACE' ) );
#6349 = CARTESIAN_POINT ( 'NONE',  ( 0.000000000000000000, -9.999999999999998224, 2.750000000000000000 ) ) ;
#6350 = DIRECTION ( 'NONE',  ( 0.000000000000000000, 0.9925461516413219831, -0.1218693434051477398 ) ) ;
#6351 = CARTESIAN_POINT ( 'NONE',  ( -5.385316468750001029, -27.13020833299193413, -3.109213912904136734 ) ) ;
#6352 = CARTESIAN_POINT ( 'NONE',  ( -2.557341765625002594, -28.94270833367473017, 4.429445870380399164 ) ) ;
#6353 = CYLINDRICAL_SURFACE ( 'NONE', #2118, 4.000000000000000000 ) ;
#6354 = CARTESIAN_POINT ( 'NONE',  ( 3.220014416085498963E-16, -29.00000000000000355, 2.629341307491595447 ) ) ;
#6355 = CARTESIAN_POINT ( 'NONE',  ( 1.224499502706077214, -7.149340926099361226, 3.007514324621463508 ) ) ;
#6356 = CARTESIAN_POINT ( 'NONE',  ( -1.975475456537005874E-15, -28.09375000068279604, 5.250000000000000000 ) ) ;
#6357 = CARTESIAN_POINT ( 'NONE',  ( -2.692658234375000514, -28.40104166632526628, -4.663820869356205989 ) ) ;
#6358 = CARTESIAN_POINT ( 'NONE',  ( -4.007514324621431534, -2.850659073900638774, -1.638713065079248521 ) ) ;
#6359 = DIRECTION ( 'NONE',  ( 0.000000000000000000, 0.000000000000000000, -1.000000000000000000 ) ) ;
#6360 = VECTOR ( 'NONE', #6932, 1000.000000000000000 ) ;
#6361 = CARTESIAN_POINT ( 'NONE',  ( -1.406733260263393293, -26.95758545099816672, -5.250000000000000000 ) ) ;
#6362 = ORIENTED_EDGE ( 'NONE', *, *, #4871, .T. ) ;
#6363 = CARTESIAN_POINT ( 'NONE',  ( -5.250000000000000000, -29.52083333333333215, -3.031088913245534755 ) ) ;
#6364 = CIRCLE ( 'NONE', #7571, 5.242490174541154069 ) ;
#6365 = CARTESIAN_POINT ( 'NONE',  ( -5.114683531250000748, -27.48437500034139802, -6.263680815196995234E-16 ) ) ;
#6366 = CARTESIAN_POINT ( 'NONE',  ( -3.000000000000000444, 0.2493409260993606213, 0.01814118441314532468 ) ) ;
#6367 = CARTESIAN_POINT ( 'NONE',  ( 5.249999999999999112, -29.52083333333333215, 3.031088913245538308 ) ) ;
#6368 = CARTESIAN_POINT ( 'NONE',  ( 1.406733260263403507, -29.32366454968462932, -5.249999999999994671 ) ) ;
#6369 = CARTESIAN_POINT ( 'NONE',  ( 2.557341765625000818, -29.38020833367473017, -4.429445870380400052 ) ) ;
#6370 = CARTESIAN_POINT ( 'NONE',  ( -5.114683531250000748, -27.04687500034139802, -6.263680815196995234E-16 ) ) ;
#6371 = CIRCLE ( 'NONE', #1194, 1.499999999999999778 ) ;
#6372 = CARTESIAN_POINT ( 'NONE',  ( -5.249999999999999112, -28.42708333401612819, -3.031088913245536975 ) ) ;
#6373 = CARTESIAN_POINT ( 'NONE',  ( -2.625000000000000444, -28.97916666598386826, -4.546633369868303021 ) ) ;
#6374 = CARTESIAN_POINT ( 'NONE',  ( -1.000000000000000000, -29.00000000000000355, -3.048902179152658931 ) ) ;
#6375 = CARTESIAN_POINT ( 'NONE',  ( -2.214270216908088340, -1.191525181865939160E-11, 2.839183589524241658 ) ) ;
#6376 = FACE_BOUND ( 'NONE', #7465, .T. ) ;
#6377 = CARTESIAN_POINT ( 'NONE',  ( -2.557341765624999042, -29.83854166700806232, -4.429445870380400052 ) ) ;
#6378 = CARTESIAN_POINT ( 'NONE',  ( -3.492485675378536047, -6.549340926099363358, -1.467888652719048670 ) ) ;
#6379 = EDGE_CURVE ( 'NONE', #7379, #6698, #6621, .T. ) ;
#6380 = ORIENTED_EDGE ( 'NONE', *, *, #3497, .T. ) ;
#6381 = DIRECTION ( 'NONE',  ( 0.000000000000000000, -1.000000000000000000, 0.000000000000000000 ) ) ;
#6382 = CIRCLE ( 'NONE', #2980, 2.000000000000000000 ) ;
#6383 = CARTESIAN_POINT ( 'NONE',  ( 5.114683531250000748, -29.60937500034139802, 0.000000000000000000 ) ) ;
#6384 =( BOUNDED_CURVE ( )  B_SPLINE_CURVE ( 2, ( #4117, #3425, #4529, #984, #5217, #7217, #7265, #6564, #3000 ),
 .UNSPECIFIED., .F., .F. ) 
 B_SPLINE_CURVE_WITH_KNOTS ( ( 3, 2, 2, 2, 3 ),
 ( 0.3125000000000000000, 0.3194444444444444198, 0.3333333333333333148, 0.3472222222222222099, 0.3541666666666666297 ),
 .UNSPECIFIED. ) 
 CURVE ( )  GEOMETRIC_REPRESENTATION_ITEM ( )  RATIONAL_B_SPLINE_CURVE ( ( 0.9330127018922194093, 0.9330127018922194093, 1.000000000000000000, 0.8660254037844387076, 1.000000000000000000, 0.8660254037844387076, 1.000000000000000000, 0.9330127018922196314, 0.9330127018922194093 ) ) 
 REPRESENTATION_ITEM ( '' )  );
#6385 = ADVANCED_FACE ( 'NONE', ( #3009 ), #1699, .T. ) ;
#6386 = ORIENTED_EDGE ( 'NONE', *, *, #5647, .T. ) ;
#6387 = ORIENTED_EDGE ( 'NONE', *, *, #1607, .F. ) ;
#6388 = CARTESIAN_POINT ( 'NONE',  ( 0.000000000000000000, 75.00000000000000000, -2.499999999999999556 ) ) ;
#6389 = CARTESIAN_POINT ( 'NONE',  ( 1.467888652718972731, -6.650659073900639484, 3.492485675378566246 ) ) ;
#6390 = DIRECTION ( 'NONE',  ( -0.000000000000000000, -1.000000000000000000, -0.000000000000000000 ) ) ;
#6391 = VECTOR ( 'NONE', #1606, 1000.000000000000000 ) ;
#6392 = EDGE_CURVE ( 'NONE', #4680, #784, #2256, .T. ) ;
#6393 = EDGE_LOOP ( 'NONE', ( #5036, #7164, #8692, #7547, #5558, #5603, #2629, #6811 ) ) ;
#6394 = LINE ( 'NONE', #29, #5051 ) ;
#6395 = DIRECTION ( 'NONE',  ( 0.000000000000000000, -0.000000000000000000, -1.000000000000000000 ) ) ;
#6396 = CARTESIAN_POINT ( 'NONE',  ( 2.692658234374998738, -27.19270833299193413, -4.663820869356206877 ) ) ;
#6397 = CARTESIAN_POINT ( 'NONE',  ( -5.114683531250000748, -28.48437500034139802, -6.263680815196995234E-16 ) ) ;
#6398 = CARTESIAN_POINT ( 'NONE',  ( -3.507514324621464397, -1.949340926099361271, 1.431606283892619347 ) ) ;
#6399 = ITEM_DEFINED_TRANSFORMATION ( 'NONE', 'NONE', #2658,  #888 ) ;
#6400 = PLANE ( 'NONE',  #8231 ) ;
#6401 = CARTESIAN_POINT ( 'NONE',  ( -3.007514324621463508, -1.949340926099361493, 1.224499502706077658 ) ) ;
#6402 = FACE_OUTER_BOUND ( 'NONE', #2114, .T. ) ;
#6403 = CARTESIAN_POINT ( 'NONE',  ( 5.385316468750000141, -28.48437499965860198, -6.595110575850215044E-16 ) ) ;
#6404 = CARTESIAN_POINT ( 'NONE',  ( 1.674995433905515085, -1.850659073900638774, 3.992485675378568022 ) ) ;
#6405 = FILL_AREA_STYLE ('',( #5580 ) ) ;
#6406 = ADVANCED_FACE ( 'NONE', ( #5925 ), #993, .T. ) ;
#6407 = ORIENTED_EDGE ( 'NONE', *, *, #2018, .F. ) ;
#6408 = CARTESIAN_POINT ( 'NONE',  ( 2.692658234374998738, -27.41145833299193413, -4.663820869356206877 ) ) ;
#6409 = EDGE_LOOP ( 'NONE', ( #3729, #6835 ) ) ;
#6410 = CARTESIAN_POINT ( 'NONE',  ( -2.692658234374996518, -27.53645833299193413, 4.663820869356208654 ) ) ;
#6411 = CARTESIAN_POINT ( 'NONE',  ( -2.992485675378564469, 0.1493409260993606713, 1.260781871532430820 ) ) ;
#6412 = ORIENTED_EDGE ( 'NONE', *, *, #2832, .T. ) ;
#6413 = CARTESIAN_POINT ( 'NONE',  ( -2.625000000000002220, -29.33333333333333215, 4.546633369868302132 ) ) ;
#6414 = CARTESIAN_POINT ( 'NONE',  ( 1.000000000000000000, -29.00000000000000355, 2.431755684948965435 ) ) ;
#6415 = CARTESIAN_POINT ( 'NONE',  ( -5.114683531250000748, -27.81770833367473017, -2.952963913586935440 ) ) ;
#6416 = VECTOR ( 'NONE', #4784, 1000.000000000000000 ) ;
#6417 = VECTOR ( 'NONE', #1591, 1000.000000000000227 ) ;
#6418 = CARTESIAN_POINT ( 'NONE',  ( 5.114683531249999859, -27.90104166700806587, -2.952963913586932776 ) ) ;
#6419 = DIRECTION ( 'NONE',  ( 0.000000000000000000, -1.000000000000000000, 0.000000000000000000 ) ) ;
#6420 = CARTESIAN_POINT ( 'NONE',  ( 0.000000000000000000, -27.00000000000000000, 0.000000000000000000 ) ) ;
#6421 = CARTESIAN_POINT ( 'NONE',  ( -3.750000000000000000, 0.000000000000000000, -3.927886379372531234E-14 ) ) ;
#6422 = VECTOR ( 'NONE', #3440, 1000.000000000000000 ) ;
#6423 = CARTESIAN_POINT ( 'NONE',  ( 2.625000000000000444, -28.45833333333333215, -4.546633369868303021 ) ) ;
#6424 = DIRECTION ( 'NONE',  ( 0.000000000000000000, 0.9925461516413219831, -0.1218693434051477398 ) ) ;
#6425 = CARTESIAN_POINT ( 'NONE',  ( 2.462045979635577364, -7.249340926099360871, 2.487701488670255312 ) ) ;
#6426 = ORIENTED_EDGE ( 'NONE', *, *, #1184, .F. ) ;
#6427 = CARTESIAN_POINT ( 'NONE',  ( 5.250000000000000888, -28.08333333265053255, 3.031088913245533423 ) ) ;
#6428 = CARTESIAN_POINT ( 'NONE',  ( -1.406733260263391960, -28.88616454900183328, 5.250000000000000000 ) ) ;
#6429 = CARTESIAN_POINT ( 'NONE',  ( 5.249999999999999112, -27.05208333401612819, 3.031088913245538308 ) ) ;
#6430 = VERTEX_POINT ( 'NONE', #5833 ) ;
#6431 = CIRCLE ( 'NONE', #2441, 1.750000000000000222 ) ;
#6432 = EDGE_LOOP ( 'NONE', ( #3647, #6982, #8902 ) ) ;
#6433 = DIRECTION ( 'NONE',  ( 0.000000000000000000, 0.000000000000000000, -1.000000000000000000 ) ) ;
#6434 = CARTESIAN_POINT ( 'NONE',  ( 1.431606283892694842, -5.650659073900638596, -3.507514324621434199 ) ) ;
#6435 = CARTESIAN_POINT ( 'NONE',  ( 6.972266317189433020E-16, -27.18750000000000000, -5.250000000000000000 ) ) ;
#6436 = ORIENTED_EDGE ( 'NONE', *, *, #1335, .T. ) ;
#6437 =( BOUNDED_CURVE ( )  B_SPLINE_CURVE ( 2, ( #8766, #113, #7227, #5970, #8674, #854, #3653, #3010, #2209, #8070, #7936, #2397, #6478, #951, #2962, #1700, #5226, #4353, #3701, #5033, #3800, #4441, #6667, #4537, #6577, #5834, #7370, #7188, #994, #4492, #2306, #1600, #8626, #5128, #7278, #3752, #904, #210, #2257, #7890, #3060, #1653, #6623, #7324, #5880, #5082, #8717, #2349, #3152, #5179, #250, #8943, #2594, #3334, #439, #8168, #3238, #7420, #8118, #1044, #1937, #6864, #2542, #7609, #6016, #4719, #8811, #4629, #4074, #8213, #488, #7559, #1796, #6062, #7512, #1186, #4030, #4765, #3892, #6164, #1847, #6813, #8898, #8990, #1747, #5274, #5365, #4583, #5412, #6115, #2639, #4675, #6911, #1233, #5460, #535, #3376, #1893, #8305, #1095, #7467, #6763, #2448, #3936, #2493, #6712, #342, #3195, #1141, #8261, #8854, #5315, #390, #3983, #3286, #6951, #2725, #7610, #3239, #6912, #489, #4116, #580, #5366, #536, #3287, #1096, #7655, #8215, #1234, #6210, #7513, #4075, #3377, #2595, #3937, #3424, #8262, #1278, #9039, #8354, #6063, #5413, #8398, #6253 ),
 .UNSPECIFIED., .F., .T. ) 
 B_SPLINE_CURVE_WITH_KNOTS ( ( 3, 2, 2, 2, 2, 2, 2, 2, 2, 2, 2, 2, 2, 2, 2, 2, 2, 2, 2, 2, 2, 2, 2, 2, 2, 2, 2, 2, 2, 2, 2, 2, 2, 2, 2, 2, 2, 2, 2, 2, 2, 2, 2, 2, 2, 2, 2, 2, 2, 2, 2, 2, 2, 2, 2, 2, 2, 2, 2, 2, 2, 2, 2, 2, 2, 2, 2, 2, 2, 2, 2, 2, 3 ),
 ( 0.000000000000000000, 0.01388888888888888812, 0.02777777777777777624, 0.04166666666666666435, 0.05555555555555555247, 0.06944444444444444753, 0.08333333333333332871, 0.09722222222222222376, 0.1111111111111111049, 0.1250000000000000000, 0.1388888888888888951, 0.1527777777777777901, 0.1666666666666666574, 0.1805555555555555525, 0.1944444444444444475, 0.2083333333333333426, 0.2222222222222222099, 0.2361111111111111049, 0.2500000000000000000, 0.2638888888888888951, 0.2777777777777777901, 0.2916666666666666852, 0.3055555555555555802, 0.3194444444444444198, 0.3333333333333333148, 0.3472222222222222099, 0.3611111111111111049, 0.3750000000000000000, 0.3888888888888888951, 0.4027777777777777901, 0.4166666666666666852, 0.4305555555555555802, 0.4444444444444444198, 0.4583333333333333148, 0.4722222222222222099, 0.4861111111111111049, 0.5000000000000000000, 0.5138888888888888395, 0.5277777777777777901, 0.5416666666666666297, 0.5555555555555555802, 0.5694444444444444198, 0.5833333333333333703, 0.5972222222222222099, 0.6111111111111111605, 0.6250000000000000000, 0.6388888888888888395, 0.6527777777777777901, 0.6666666666666666297, 0.6805555555555555802, 0.6944444444444444198, 0.7083333333333333703, 0.7222222222222222099, 0.7361111111111111605, 0.7500000000000000000, 0.7638888888888888395, 0.7777777777777777901, 0.7916666666666666297, 0.8055555555555555802, 0.8194444444444444198, 0.8333333333333333703, 0.8472222222222222099, 0.8611111111111111605, 0.8750000000000000000, 0.8888888888888888395, 0.9027777777777777901, 0.9166666666666666297, 0.9305555555555555802, 0.9444444444444444198, 0.9583333333333333703, 0.9722222222222222099, 0.9861111111111111605, 1.000000000000000000 ),
 .UNSPECIFIED. ) 
 CURVE ( )  GEOMETRIC_REPRESENTATION_ITEM ( )  RATIONAL_B_SPLINE_CURVE ( ( 1.000000000000000000, 0.8660254037844387076, 1.000000000000000000, 0.8660254037844387076, 1.000000000000000000, 0.8660254037844387076, 1.000000000000000000, 0.8660254037844387076, 1.000000000000000000, 0.8660254037844387076, 1.000000000000000000, 0.8660254037844387076, 1.000000000000000000, 0.8660254037844387076, 1.000000000000000000, 0.8660254037844387076, 1.000000000000000000, 0.8660254037844387076, 1.000000000000000000, 0.8660254037844387076, 1.000000000000000000, 0.8660254037844387076, 1.000000000000000000, 0.8660254037844387076, 1.000000000000000000, 0.8660254037844387076, 1.000000000000000000, 0.8660254037844387076, 1.000000000000000000, 0.8660254037844387076, 1.000000000000000000, 0.8660254037844387076, 1.000000000000000000, 0.8660254037844387076, 1.000000000000000000, 0.8660254037844387076, 1.000000000000000000, 0.8660254037844387076, 1.000000000000000000, 0.8660254037844387076, 1.000000000000000000, 0.8660254037844387076, 1.000000000000000000, 0.8660254037844387076, 1.000000000000000000, 0.8660254037844387076, 1.000000000000000000, 0.8660254037844387076, 1.000000000000000000, 0.8660254037844387076, 1.000000000000000000, 0.8660254037844387076, 1.000000000000000000, 0.8660254037844387076, 1.000000000000000000, 0.8660254037844387076, 1.000000000000000000, 0.8660254037844387076, 1.000000000000000000, 0.8660254037844387076, 1.000000000000000000, 0.8660254037844387076, 1.000000000000000000, 0.8660254037844387076, 1.000000000000000000, 0.8660254037844387076, 1.000000000000000000, 0.8660254037844387076, 1.000000000000000000, 0.8660254037844387076, 1.000000000000000000, 0.8660254037844387076, 1.000000000000000000, 0.8660254037844387076, 1.000000000000000000, 0.8660254037844387076, 1.000000000000000000, 0.8660254037844387076, 1.000000000000000000, 0.8660254037844387076, 1.000000000000000000, 0.8660254037844387076, 1.000000000000000000, 0.8660254037844387076, 1.000000000000000000, 0.8660254037844387076, 1.000000000000000000, 0.8660254037844387076, 1.000000000000000000, 0.8660254037844387076, 1.000000000000000000, 0.8660254037844387076, 1.000000000000000000, 0.8660254037844387076, 1.000000000000000000, 0.8660254037844387076, 1.000000000000000000, 0.8660254037844387076, 1.000000000000000000, 0.8660254037844387076, 1.000000000000000000, 0.8660254037844387076, 1.000000000000000000, 0.8660254037844387076, 1.000000000000000000, 0.8660254037844387076, 1.000000000000000000, 0.8660254037844387076, 1.000000000000000000, 0.8660254037844387076, 1.000000000000000000, 0.8660254037844387076, 1.000000000000000000, 0.8660254037844387076, 1.000000000000000000, 0.8660254037844387076, 1.000000000000000000, 0.8660254037844387076, 1.000000000000000000, 0.8660254037844387076, 1.000000000000000000, 0.8660254037844387076, 1.000000000000000000, 0.8660254037844387076, 1.000000000000000000, 0.8660254037844387076, 1.000000000000000000, 0.8660254037844387076, 1.000000000000000000, 0.8660254037844387076, 1.000000000000000000, 0.8660254037844387076, 1.000000000000000000, 0.8660254037844387076, 1.000000000000000000, 0.8660254037844387076, 1.000000000000000000, 0.8660254037844387076, 1.000000000000000000, 0.8660254037844387076, 1.000000000000000000, 0.8660254037844387076, 1.000000000000000000, 0.8660254037844387076, 1.000000000000000000 ) ) 
 REPRESENTATION_ITEM ( '' )  );
#6438 = ADVANCED_FACE ( 'NONE', ( #5080 ), #2604, .T. ) ;
#6439 = CARTESIAN_POINT ( 'NONE',  ( -5.249999999999999112, -29.02083333333332860, -3.031088913245534755 ) ) ;
#6440 = CARTESIAN_POINT ( 'NONE',  ( 0.000000000000000000, -20.00000000000000000, 0.000000000000000000 ) ) ;
#6441 = CARTESIAN_POINT ( 'NONE',  ( 5.249999999999999112, -27.76041666734946389, -3.031088913245534755 ) ) ;
#6442 = CARTESIAN_POINT ( 'NONE',  ( -1.084901341431563923E-15, -27.92187500034139802, 5.905927827173866440 ) ) ;
#6443 = DIRECTION ( 'NONE',  ( 0.000000000000000000, 0.000000000000000000, 1.000000000000000000 ) ) ;
#6444 = DIRECTION ( 'NONE',  ( 0.000000000000000000, -0.000000000000000000, 1.000000000000000000 ) ) ;
#6445 = CARTESIAN_POINT ( 'NONE',  ( -1.260781871532494103, -5.349340926099361404, 2.992485675378538712 ) ) ;
#6446 = DIRECTION ( 'NONE',  ( 1.039441819132096507E-14, 0.07256473765270715637, -0.9973637043974449279 ) ) ;
#6447 = CARTESIAN_POINT ( 'NONE',  ( -3.807688866302469071E-16, -27.42187499965860198, -6.218427825808274356 ) ) ;
#6448 = CARTESIAN_POINT ( 'NONE',  ( 1.674995433905515085, -6.650659073900639484, 3.992485675378568022 ) ) ;
#6449 = EDGE_CURVE ( 'NONE', #6852, #6768, #6158, .T. ) ;
#6450 = DIRECTION ( 'NONE',  ( -0.000000000000000000, -1.000000000000000000, -0.000000000000000000 ) ) ;
#6451 = CYLINDRICAL_SURFACE ( 'NONE', #4898, 5.250000000000000000 ) ;
#6452 = EDGE_LOOP ( 'NONE', ( #6795, #6648, #460, #3941 ) ) ;
#6453 = CARTESIAN_POINT ( 'NONE',  ( 1.113604000661152470E-15, -29.43750000000000000, 6.062177826491070398 ) ) ;
#6454 = VERTEX_POINT ( 'NONE', #5783 ) ;
#6455 = CARTESIAN_POINT ( 'NONE',  ( 5.385316468749999252, -27.43229166632526983, -3.109213912904139399 ) ) ;
#6456 = CARTESIAN_POINT ( 'NONE',  ( -2.108492589042352261, -6.350659073900638774, 2.134148098076933397 ) ) ;
#6457 = EDGE_CURVE ( 'NONE', #7180, #2870, #7041, .T. ) ;
#6458 = EDGE_LOOP ( 'NONE', ( #3236, #1035, #8671, #927, #4684, #6470, #8151, #2254, #2236, #4556, #8403, #3521, #4633, #6219, #3601, #3271, #437, #3650, #4969, #5290, #7396, #8925, #6097, #2648, #6677, #949, #307, #3867 ) ) ;
#6459 = CARTESIAN_POINT ( 'NONE',  ( -5.250000000000000888, -28.60416666666666430, 3.031088913245532979 ) ) ;
#6460 = DIRECTION ( 'NONE',  ( 0.000000000000000000, 0.000000000000000000, -1.000000000000000000 ) ) ;
#6461 =( BOUNDED_CURVE ( )  B_SPLINE_CURVE ( 2, ( #1764, #7437, #7245, #1668, #4511 ),
 .UNSPECIFIED., .F., .F. ) 
 B_SPLINE_CURVE_WITH_KNOTS ( ( 3, 2, 3 ),
 ( 0.000000000000000000, 0.01388888888888888812, 0.02083333333333333218 ),
 .UNSPECIFIED. ) 
 CURVE ( )  GEOMETRIC_REPRESENTATION_ITEM ( )  RATIONAL_B_SPLINE_CURVE ( ( 1.000000000000000000, 0.8660254037844387076, 1.000000000000000000, 0.9330127018922194093, 0.9330127018922194093 ) ) 
 REPRESENTATION_ITEM ( '' )  );
#6462 = CARTESIAN_POINT ( 'NONE',  ( 2.557341765625000818, -27.38020833367473017, -4.429445870380400052 ) ) ;
#6463 = CARTESIAN_POINT ( 'NONE',  ( -2.557341765625002594, -28.25520833367473017, 4.429445870380399164 ) ) ;
#6464 = CARTESIAN_POINT ( 'NONE',  ( 0.000000000000000000, -20.00000000000000000, -2.000000000000000000 ) ) ;
#6465 = DIRECTION ( 'NONE',  ( 1.000000000000000000, 0.000000000000000000, 0.000000000000000000 ) ) ;
#6466 = DIRECTION ( 'NONE',  ( 0.000000000000000000, 1.000000000000000000, 0.000000000000000000 ) ) ;
#6467 = CARTESIAN_POINT ( 'NONE',  ( -1.000000000000000000, -29.00000000000000355, 2.431755684948965435 ) ) ;
#6468 = CARTESIAN_POINT ( 'NONE',  ( -5.114683531250000748, -29.79687500034139802, -6.263680815196995234E-16 ) ) ;
#6469 = CARTESIAN_POINT ( 'NONE',  ( 1.431606283892619125, -5.549340926099361582, 3.507514324621464397 ) ) ;
#6470 = ORIENTED_EDGE ( 'NONE', *, *, #6337, .F. ) ;
#6471 = LINE ( 'NONE', #7971, #7597 ) ;
#6472 = CARTESIAN_POINT ( 'NONE',  ( 2.625000000000000444, -27.95833333333333215, -4.546633369868303021 ) ) ;
#6473 = CARTESIAN_POINT ( 'NONE',  ( 3.616337804771879580E-16, -27.79687500034139802, -5.905927827173866440 ) ) ;
#6474 = VERTEX_POINT ( 'NONE', #3935 ) ;
#6475 = ADVANCED_FACE ( 'NONE', ( #2447 ), #3237, .T. ) ;
#6476 = ORIENTED_EDGE ( 'NONE', *, *, #2018, .T. ) ;
#6477 = CARTESIAN_POINT ( 'NONE',  ( 5.250000000000000888, -29.64583333333333215, 3.031088913245533423 ) ) ;
#6478 = CARTESIAN_POINT ( 'NONE',  ( -5.385316468750000141, -27.35937499965860198, 0.000000000000000000 ) ) ;
#6479 = CARTESIAN_POINT ( 'NONE',  ( 2.815599370228907716, -2.350659073900638774, -2.841254879263473310 ) ) ;
#6480 = PRESENTATION_STYLE_ASSIGNMENT (( #162 ) ) ;
#6481 = ORIENTED_EDGE ( 'NONE', *, *, #7313, .T. ) ;
#6482 = CARTESIAN_POINT ( 'NONE',  ( 6.972266317189433020E-16, -29.93750000000000000, -5.250000000000000000 ) ) ;
#6483 = CARTESIAN_POINT ( 'NONE',  ( 5.249999999999999112, -29.05208333401612819, 3.031088913245538308 ) ) ;
#6484 =( GEOMETRIC_REPRESENTATION_CONTEXT ( 3 ) GLOBAL_UNCERTAINTY_ASSIGNED_CONTEXT ( ( #4405 ) ) GLOBAL_UNIT_ASSIGNED_CONTEXT ( ( #6796, #8248, #4795 ) ) REPRESENTATION_CONTEXT ( 'NONE', 'WORKASPACE' ) );
#6485 = FACE_OUTER_BOUND ( 'NONE', #5254, .T. ) ;
#6486 = CARTESIAN_POINT ( 'NONE',  ( -2.557341765625002594, -26.94270833367473017, 4.429445870380399164 ) ) ;
#6487 = CARTESIAN_POINT ( 'NONE',  ( -1.431606283892620235, -1.549340926099361138, -3.507514324621463953 ) ) ;
#6488 = DIRECTION ( 'NONE',  ( -0.000000000000000000, -1.000000000000000000, -0.000000000000000000 ) ) ;
#6489 = CARTESIAN_POINT ( 'NONE',  ( -2.108492589042306964, -1.649340926099361448, -2.134148098076978251 ) ) ;
#6490 = CARTESIAN_POINT ( 'NONE',  ( -5.249999999999999112, -28.17708333401612819, -3.031088913245536975 ) ) ;
#6491 = PRESENTATION_LAYER_ASSIGNMENT (  '', '', ( #4576 ) ) ;
#6492 = CARTESIAN_POINT ( 'NONE',  ( 5.385316468750000141, -27.98437499965860198, -6.595110575850215044E-16 ) ) ;
#6493 = CARTESIAN_POINT ( 'NONE',  ( -2.815599370228846876, -4.849340926099359628, -2.841254879263533262 ) ) ;
#6494 = DIRECTION ( 'NONE',  ( 0.000000000000000000, -0.000000000000000000, 1.000000000000000000 ) ) ;
#6495 = DIRECTION ( 'NONE',  ( 0.000000000000000000, 1.000000000000000000, 0.000000000000000000 ) ) ;
#6496 = ORIENTED_EDGE ( 'NONE', *, *, #2568, .T. ) ;
#6497 = SURFACE_STYLE_FILL_AREA ( #7728 ) ;
#6498 = CARTESIAN_POINT ( 'NONE',  ( -3.807688866302469071E-16, -27.89062499965860198, -6.218427825808274356 ) ) ;
#6499 = VERTEX_POINT ( 'NONE', #4582 ) ;
#6500 = CARTESIAN_POINT ( 'NONE',  ( 2.692658234374998738, -27.66145833299193413, -4.663820869356206877 ) ) ;
#6501 = CARTESIAN_POINT ( 'NONE',  ( -3.007514324621435531, -4.450659073900640195, -1.224499502706142273 ) ) ;
#6502 = VERTEX_POINT ( 'NONE', #1140 ) ;
#6503 = CARTESIAN_POINT ( 'NONE',  ( -5.250000000000000000, -29.12499999999999645, -6.429395695523604153E-16 ) ) ;
#6504 = CIRCLE ( 'NONE', #7258, 5.250000000000000000 ) ;
#6505 = CARTESIAN_POINT ( 'NONE',  ( 1.406733260263391960, -29.80133545031536713, 5.250000000000000000 ) ) ;
#6506 = EDGE_CURVE ( 'NONE', #946, #2693, #7702, .T. ) ;
#6507 = CARTESIAN_POINT ( 'NONE',  ( 2.557341765625000818, -28.13020833367473017, -4.429445870380400052 ) ) ;
#6508 =( NAMED_UNIT ( * ) SI_UNIT ( $, .STERADIAN. ) SOLID_ANGLE_UNIT ( ) );
#6509 = VECTOR ( 'NONE', #8540, 1000.000000000000000 ) ;
#6510 = CARTESIAN_POINT ( 'NONE',  ( 2.557341765625000818, -27.38020833367473017, -4.429445870380400052 ) ) ;
#6511 = DIRECTION ( 'NONE',  ( 0.000000000000000000, 0.000000000000000000, 1.000000000000000000 ) ) ;
#6512 = CARTESIAN_POINT ( 'NONE',  ( -2.487701488670255312, -5.249340926099360871, 2.462045979635577808 ) ) ;
#6513 = DIRECTION ( 'NONE',  ( 0.000000000000000000, -0.000000000000000000, 1.000000000000000000 ) ) ;
#6514 = CARTESIAN_POINT ( 'NONE',  ( 0.000000000000000000, 1.000000000000000000, 0.000000000000000000 ) ) ;
#6515 = CARTESIAN_POINT ( 'NONE',  ( -3.507514324621464397, -6.749340926099361759, 1.431606283892619347 ) ) ;
#6516 =( BOUNDED_CURVE ( )  B_SPLINE_CURVE ( 2, ( #1825, #280, #1025, #5956, #7402, #2625, #5256, #420, #4613, #8102, #3875, #979, #1170, #4013, #5299, #8839, #8976, #2576, #7499, #6794, #8197, #8150, #1729, #3920, #6848, #5443, #6747, #4704, #4566, #2476, #3825, #1778, #7452, #6651, #6044, #8289, #470, #8880, #3266, #4525, #1126, #5394, #6096, #8245, #8795, #2668, #7594, #5490, #1922, #4749, #1219, #4059, #6194, #6895, #522, #3364, #9022, #804, #7221, #758, #5777, #2913, #5827, #6568, #6042, #4299, #2299, #5730, #155, #203, #897, #6520, #1454, #5026, #1551, #8879, #2522, #6745, #8619 ),
 .UNSPECIFIED., .F., .F. ) 
 B_SPLINE_CURVE_WITH_KNOTS ( ( 3, 2, 2, 2, 2, 2, 2, 2, 2, 2, 2, 2, 2, 2, 2, 2, 2, 2, 2, 2, 2, 2, 2, 2, 2, 2, 2, 2, 2, 2, 2, 2, 2, 2, 2, 2, 2, 2, 2, 3 ),
 ( 0.03135029301116579181, 0.05000000000000000278, 0.07499999999999999722, 0.1000000000000000056, 0.1250000000000000000, 0.1499999999999999944, 0.1749999999999999889, 0.2000000000000000111, 0.2250000000000000056, 0.2500000000000000000, 0.2750000000000000222, 0.2999999999999999334, 0.3249999999999999556, 0.3499999999999999778, 0.3750000000000000000, 0.4000000000000000222, 0.4249999999999999334, 0.4499999999999999556, 0.4749999999999999778, 0.5000000000000000000, 0.5250000000000000222, 0.5500000000000000444, 0.5749999999999999556, 0.5999999999999999778, 0.6250000000000000000, 0.6499999999999999112, 0.6750000000000000444, 0.6999999999999999556, 0.7249999999999999778, 0.7500000000000000000, 0.7750000000000000222, 0.8000000000000000444, 0.8249999999999999556, 0.8499999999999999778, 0.8750000000000000000, 0.8999999999999999112, 0.9250000000000000444, 0.9499999999999999556, 0.9749999999999999778, 1.000000000000000000 ),
 .UNSPECIFIED. ) 
 CURVE ( )  GEOMETRIC_REPRESENTATION_ITEM ( )  RATIONAL_B_SPLINE_CURVE ( ( 0.9711519008064275482, 0.9432150234192966387, 1.000000000000000000, 0.9238795325112867385, 1.000000000000000000, 0.9238795325112867385, 1.000000000000000000, 0.9238795325112867385, 1.000000000000000000, 0.9238795325112867385, 1.000000000000000000, 0.9238795325112867385, 1.000000000000000000, 0.9238795325112867385, 1.000000000000000000, 0.9238795325112867385, 1.000000000000000000, 0.9238795325112867385, 1.000000000000000000, 0.9238795325112867385, 1.000000000000000000, 0.9238795325112867385, 1.000000000000000000, 0.9238795325112867385, 1.000000000000000000, 0.9238795325112867385, 1.000000000000000000, 0.9238795325112867385, 1.000000000000000000, 0.9238795325112867385, 1.000000000000000000, 0.9238795325112867385, 1.000000000000000000, 0.9238795325112867385, 1.000000000000000000, 0.9238795325112867385, 1.000000000000000000, 0.9238795325112867385, 1.000000000000000000, 0.9238795325112867385, 1.000000000000000000, 0.9238795325112867385, 1.000000000000000000, 0.9238795325112867385, 1.000000000000000000, 0.9238795325112867385, 1.000000000000000000, 0.9238795325112867385, 1.000000000000000000, 0.9238795325112867385, 1.000000000000000000, 0.9238795325112867385, 1.000000000000000000, 0.9238795325112867385, 1.000000000000000000, 0.9238795325112867385, 1.000000000000000000, 0.9238795325112867385, 1.000000000000000000, 0.9238795325112867385, 1.000000000000000000, 0.9238795325112867385, 1.000000000000000000, 0.9238795325112867385, 1.000000000000000000, 0.9238795325112867385, 1.000000000000000000, 0.9238795325112867385, 1.000000000000000000, 0.9238795325112867385, 1.000000000000000000, 0.9238795325112867385, 1.000000000000000000, 0.9238795325112867385, 1.000000000000000000, 0.9238795325112867385, 1.000000000000000000, 0.9238795325112867385, 1.000000000000000000 ) ) 
 REPRESENTATION_ITEM ( '' )  );
#6517 = CARTESIAN_POINT ( 'NONE',  ( 5.249999999999997335, -28.30208333401612819, 3.031088913245538308 ) ) ;
#6518 = ORIENTED_EDGE ( 'NONE', *, *, #8818, .T. ) ;
#6519 = PRESENTATION_LAYER_ASSIGNMENT (  '', '', ( #5632 ) ) ;
#6520 = CARTESIAN_POINT ( 'NONE',  ( 3.492485675378566690, -7.050659073900639839, -1.467888652718972287 ) ) ;
#6521 = CARTESIAN_POINT ( 'NONE',  ( 5.249999999999997335, -28.02083333333333215, 3.031088913245538308 ) ) ;
#6522 = CARTESIAN_POINT ( 'NONE',  ( 5.114683531250000748, -29.10937500034139802, 0.000000000000000000 ) ) ;
#6523 = VERTEX_POINT ( 'NONE', #6061 ) ;
#6524 = ORIENTED_EDGE ( 'NONE', *, *, #8673, .T. ) ;
#6525 = AXIS2_PLACEMENT_3D ( 'NONE', #484, #8987, #2635 ) ;
#6526 = CARTESIAN_POINT ( 'NONE',  ( -9.180150650966086169E-15, -28.18749999999999645, 5.250000000000000000 ) ) ;
#6527 = CARTESIAN_POINT ( 'NONE',  ( 2.815599370228847320, -0.8493409260993607379, 2.841254879263533262 ) ) ;
#6528 = FILL_AREA_STYLE_COLOUR ( '', #1027 ) ;
#6529 = VERTEX_POINT ( 'NONE', #6015 ) ;
#6530 = AXIS2_PLACEMENT_3D ( 'NONE', #1841, #4670, #3977 ) ;
#6531 = CARTESIAN_POINT ( 'NONE',  ( 2.624999999999998668, -29.83333333333333215, -4.546633369868303021 ) ) ;
#6532 = CARTESIAN_POINT ( 'NONE',  ( -5.250000000000000000, -29.65625000068279604, -6.429395695523604153E-16 ) ) ;
#6533 = CARTESIAN_POINT ( 'NONE',  ( -5.385316468750001029, -27.63020833299193413, -3.109213912904136734 ) ) ;
#6534 = UNCERTAINTY_MEASURE_WITH_UNIT (LENGTH_MEASURE( 1.000000000000000082E-05 ), #7068, 'distance_accuracy_value', 'NONE');
#6535 = CARTESIAN_POINT ( 'NONE',  ( 5.114683531250000748, -29.92187500034139802, 0.000000000000000000 ) ) ;
#6536 = CARTESIAN_POINT ( 'NONE',  ( -3.500000000000000000, -1.849340926099361182, -0.01814118441321344033 ) ) ;
#6537 = CARTESIAN_POINT ( 'NONE',  ( 2.692658234375002735, -27.24479166632526628, 4.663820869356205101 ) ) ;
#6538 = CARTESIAN_POINT ( 'NONE',  ( -2.108492589042306964, -8.049340926099361582, -2.134148098076978251 ) ) ;
#6539 = UNCERTAINTY_MEASURE_WITH_UNIT (LENGTH_MEASURE( 1.000000000000000082E-05 ), #5818, 'distance_accuracy_value', 'NONE');
#6540 = DIRECTION ( 'NONE',  ( 0.000000000000000000, 1.000000000000000000, 0.000000000000000000 ) ) ;
#6541 = CIRCLE ( 'NONE', #4207, 5.250000000000000000 ) ;
#6542 = CARTESIAN_POINT ( 'NONE',  ( 2.815599370228847320, -4.049340926099360694, 2.841254879263533262 ) ) ;
#6543 = CARTESIAN_POINT ( 'NONE',  ( -5.250000000000000000, -28.20833333265053255, -3.031088913245534755 ) ) ;
#6544 = DIRECTION ( 'NONE',  ( -1.044949058366720058E-14, -0.07256473765270715637, 0.9973637043974449279 ) ) ;
#6545 = CARTESIAN_POINT ( 'NONE',  ( 2.487701488670255756, -4.449340926099361937, -2.462045979635577364 ) ) ;
#6546 = CARTESIAN_POINT ( 'NONE',  ( 5.249999999999999112, -29.79166666598387181, -3.031088913245536975 ) ) ;
#6547 = ORIENTED_EDGE ( 'NONE', *, *, #645, .F. ) ;
#6548 =( LENGTH_UNIT ( ) NAMED_UNIT ( * ) SI_UNIT ( .MILLI., .METRE. ) );
#6549 = CARTESIAN_POINT ( 'NONE',  ( -2.692658234374996518, -28.28645833299193413, 4.663820869356208654 ) ) ;
#6550 = ADVANCED_FACE ( 'NONE', ( #3333, #389 ), #487, .F. ) ;
#6551 = CARTESIAN_POINT ( 'NONE',  ( -2.815599370228846876, -4.849340926099359628, -2.841254879263533262 ) ) ;
#6552 = CARTESIAN_POINT ( 'NONE',  ( -5.249999999999997335, -28.47916666666666785, 3.031088913245538308 ) ) ;
#6553 = VERTEX_POINT ( 'NONE', #5273 ) ;
#6554 = CARTESIAN_POINT ( 'NONE',  ( 5.385316468750001029, -27.22395833299193413, 3.109213912904135846 ) ) ;
#6555 = CARTESIAN_POINT ( 'NONE',  ( 0.01814118441314514080, -3.350659073900639662, 3.000000000000000444 ) ) ;
#6556 = ORIENTED_EDGE ( 'NONE', *, *, #1538, .T. ) ;
#6557 = CARTESIAN_POINT ( 'NONE',  ( 5.250000000000000000, -27.75000000000000000, 0.000000000000000000 ) ) ;
#6558 = ADVANCED_FACE ( 'NONE', ( #6812 ), #8942, .F. ) ;
#6559 = CARTESIAN_POINT ( 'NONE',  ( 2.557341765624996821, -27.21354166700806587, 4.429445870380401828 ) ) ;
#6560 = SURFACE_SIDE_STYLE ('',( #4474 ) ) ;
#6561 = CARTESIAN_POINT ( 'NONE',  ( -1.975475456537005874E-15, -29.34375000068279249, 5.250000000000000000 ) ) ;
#6562 = CARTESIAN_POINT ( 'NONE',  ( -5.114683531250000748, -29.75520833367473017, -2.952963913586935440 ) ) ;
#6563 = CARTESIAN_POINT ( 'NONE',  ( -1.467888652719046449, -6.949340926099361049, 3.492485675378536047 ) ) ;
#6564 = CARTESIAN_POINT ( 'NONE',  ( 1.406733260263400176, -28.72991455036743602, -5.249999999999997335 ) ) ;
#6565 = CARTESIAN_POINT ( 'NONE',  ( -1.406733260263391960, -27.69866454968462932, 5.250000000000000000 ) ) ;
#6566 = CARTESIAN_POINT ( 'NONE',  ( -1.084901341431563923E-15, -29.73437500034140157, 5.905927827173866440 ) ) ;
#6567 = ORIENTED_EDGE ( 'NONE', *, *, #6457, .F. ) ;
#6568 = CARTESIAN_POINT ( 'NONE',  ( -3.492485675378566246, -6.250659073900640017, 1.467888652718973175 ) ) ;
#6569 = AXIS2_PLACEMENT_3D ( 'NONE', #8991, #8306, #1938 ) ;
#6570 = CARTESIAN_POINT ( 'NONE',  ( -2.625000000000002220, -29.33333333333333215, 4.546633369868302132 ) ) ;
#6571 = CARTESIAN_POINT ( 'NONE',  ( -5.114683531250000748, -28.21354166700806232, 2.952963913586931888 ) ) ;
#6572 =( REPRESENTATION_RELATIONSHIP ('NONE','NONE', #735, #1843 ) REPRESENTATION_RELATIONSHIP_WITH_TRANSFORMATION ( #6783 )SHAPE_REPRESENTATION_RELATIONSHIP( ) );
#6573 = ORIENTED_EDGE ( 'NONE', *, *, #8365, .T. ) ;
#6574 = AXIS2_PLACEMENT_3D ( 'NONE', #5795, #2927, #4953 ) ;
#6575 =( BOUNDED_CURVE ( )  B_SPLINE_CURVE ( 2, ( #5136, #8772, #6531, #857, #3156, #5279, #4543, #3756, #4498 ),
 .UNSPECIFIED., .F., .T. ) 
 B_SPLINE_CURVE_WITH_KNOTS ( ( 3, 2, 2, 2, 3 ),
 ( 0.9375000000000000000, 0.9444444444444444198, 0.9583333333333333703, 0.9722222222222222099, 0.9791666666666667407 ),
 .UNSPECIFIED. ) 
 CURVE ( )  GEOMETRIC_REPRESENTATION_ITEM ( )  RATIONAL_B_SPLINE_CURVE ( ( 0.9330127018922194093, 0.9330127018922194093, 1.000000000000000000, 0.8660254037844387076, 1.000000000000000000, 0.8660254037844387076, 1.000000000000000000, 0.9330127018922187432, 0.9330127018922192983 ) ) 
 REPRESENTATION_ITEM ( '' )  );
#6576 = CARTESIAN_POINT ( 'NONE',  ( -1.406733260263394625, -29.80133545031537068, -5.250000000000000000 ) ) ;
#6577 = CARTESIAN_POINT ( 'NONE',  ( -5.385316468750000141, -27.60937499965860198, 0.000000000000000000 ) ) ;
#6578 = CARTESIAN_POINT ( 'NONE',  ( 1.638713065079247855, -2.450659073900638862, -4.007514324621431534 ) ) ;
#6579 = COLOUR_RGB ( '',0.8941176470588234615, 0.8941176470588234615, 0.8941176470588234615 ) ;
#6580 = CARTESIAN_POINT ( 'NONE',  ( 2.300847884672513123E-14, -27.43750000000000355, -5.250000000000000000 ) ) ;
#6581 = CIRCLE ( 'NONE', #1906, 3.999999999999999112 ) ;
#6582 = ORIENTED_EDGE ( 'NONE', *, *, #8142, .F. ) ;
#6583 = FACE_BOUND ( 'NONE', #3806, .T. ) ;
#6584 = AXIS2_PLACEMENT_3D ( 'NONE', #2412, #5100, #7387 ) ;
#6585 = CARTESIAN_POINT ( 'NONE',  ( -5.250000000000000000, -29.15625000068279604, -6.429395695523604153E-16 ) ) ;
#6586 = EDGE_CURVE ( 'NONE', #8584, #2823, #1846, .T. ) ;
#6587 = CARTESIAN_POINT ( 'NONE',  ( 1.142306659890740623E-15, -27.54687499965860198, 6.218427825808274356 ) ) ;
#6588 = CARTESIAN_POINT ( 'NONE',  ( -5.114683531249999859, -27.75520833367473017, -2.952963913586935440 ) ) ;
#6589 = CARTESIAN_POINT ( 'NONE',  ( -2.462045979635576920, -1.649340926099361004, -2.487701488670255756 ) ) ;
#6590 = CARTESIAN_POINT ( 'NONE',  ( -5.385316468750000141, -27.57812499965860198, 0.000000000000000000 ) ) ;
#6591 = CARTESIAN_POINT ( 'NONE',  ( 1.260781871532495657, -7.749340926099362648, -2.992485675378538268 ) ) ;
#6592 = CARTESIAN_POINT ( 'NONE',  ( -1.406733260263402174, -29.38616454900182973, 5.249999999999995559 ) ) ;
#6593 = CARTESIAN_POINT ( 'NONE',  ( 2.815599370228847320, -0.8493409260993607379, 2.841254879263533262 ) ) ;
#6594 = AXIS2_PLACEMENT_3D ( 'NONE', #2305, #4440, #4718 ) ;
#6595 = CARTESIAN_POINT ( 'NONE',  ( -5.249999999999999112, -27.91666666598387181, 3.031088913245538308 ) ) ;
#6596 = LINE ( 'NONE', #919, #5089 ) ;
#6597 = CARTESIAN_POINT ( 'NONE',  ( -0.01814118441321365544, -5.449340926099361937, 3.500000000000000000 ) ) ;
#6598 = DIRECTION ( 'NONE',  ( -0.000000000000000000, -1.000000000000000000, -0.000000000000000000 ) ) ;
#6599 = CARTESIAN_POINT ( 'NONE',  ( -5.385316468750000141, -27.57812499965860198, 0.000000000000000000 ) ) ;
#6600 = EDGE_CURVE ( 'NONE', #5349, #2249, #3043, .T. ) ;
#6601 = CARTESIAN_POINT ( 'NONE',  ( -1.638713065079163034, -3.149340926099360782, -4.007514324621466173 ) ) ;
#6602 = FACE_OUTER_BOUND ( 'NONE', #5257, .T. ) ;
#6603 = ORIENTED_EDGE ( 'NONE', *, *, #6793, .T. ) ;
#6604 = CARTESIAN_POINT ( 'NONE',  ( -2.692658234375000514, -27.11979166632526628, -4.663820869356205989 ) ) ;
#6605 = CARTESIAN_POINT ( 'NONE',  ( 3.492485675378566690, -0.6506590739006391511, -1.467888652718972287 ) ) ;
#6606 = EDGE_LOOP ( 'NONE', ( #4700, #5060, #1139, #326 ) ) ;
#6607 = CARTESIAN_POINT ( 'NONE',  ( 5.250000000000000000, -27.25000000000000000, 0.000000000000000000 ) ) ;
#6608 = CARTESIAN_POINT ( 'NONE',  ( 2.557341765625000818, -28.38020833367473017, -4.429445870380400052 ) ) ;
#6609 = CARTESIAN_POINT ( 'NONE',  ( 1.113604000661152470E-15, -27.43750000000000000, 6.062177826491070398 ) ) ;
#6610 = DIRECTION ( 'NONE',  ( 0.000000000000000000, 0.000000000000000000, 1.000000000000000000 ) ) ;
#6611 = CARTESIAN_POINT ( 'NONE',  ( -2.462045979635576920, -3.249340926099361315, -2.487701488670255756 ) ) ;
#6612 = EDGE_CURVE ( 'NONE', #2117, #2142, #7466, .T. ) ;
#6613 = CARTESIAN_POINT ( 'NONE',  ( 0.000000000000000000, -50.00000000000000000, 0.000000000000000000 ) ) ;
#6614 = CARTESIAN_POINT ( 'NONE',  ( 2.625000000000000444, -28.70833333333333215, -4.546633369868303021 ) ) ;
#6615 = CARTESIAN_POINT ( 'NONE',  ( -5.114683531250000748, -28.29687500034139447, -6.263680815196995234E-16 ) ) ;
#6616 = CARTESIAN_POINT ( 'NONE',  ( 9.180150650966086169E-15, -28.34375000068279604, 5.250000000000000000 ) ) ;
#6617 = ORIENTED_EDGE ( 'NONE', *, *, #8913, .F. ) ;
#6618 = CARTESIAN_POINT ( 'NONE',  ( 9.180150650966086169E-15, -28.34375000068279604, 5.249999999999999112 ) ) ;
#6619 = CARTESIAN_POINT ( 'NONE',  ( -1.084901341431563923E-15, -28.42187500034139802, 5.905927827173866440 ) ) ;
#6620 = ORIENTED_EDGE ( 'NONE', *, *, #4928, .T. ) ;
#6621 = LINE ( 'NONE', #249, #3480 ) ;
#6622 = ADVANCED_FACE ( 'NONE', ( #1892 ), #1041, .T. ) ;
#6623 = CARTESIAN_POINT ( 'NONE',  ( 5.385316468750000141, -27.98437499965860198, -6.595110575850215044E-16 ) ) ;
#6624 = CARTESIAN_POINT ( 'NONE',  ( 0.01814118441313467001, -3.350659073900638774, 4.000000000000000000 ) ) ;
#6625 = CARTESIAN_POINT ( 'NONE',  ( -1.975475456537005874E-15, -29.06249999999999645, 5.250000000000000000 ) ) ;
#6626 = ORIENTED_EDGE ( 'NONE', *, *, #6672, .T. ) ;
#6627 = ADVANCED_FACE ( 'NONE', ( #5459 ), #6711, .T. ) ;
#6628 = DIRECTION ( 'NONE',  ( 0.000000000000000000, 0.000000000000000000, 1.000000000000000000 ) ) ;
#6629 = CARTESIAN_POINT ( 'NONE',  ( 3.712013335537174572E-16, -28.71875000068279604, -6.062177826491070398 ) ) ;
#6630 = CARTESIAN_POINT ( 'NONE',  ( -5.385316468750000141, -27.35937499965860198, 0.000000000000000000 ) ) ;
#6631 = CARTESIAN_POINT ( 'NONE',  ( -2.557341765625002594, -27.94270833367473017, 4.429445870380399164 ) ) ;
#6632 = ORIENTED_EDGE ( 'NONE', *, *, #4774, .T. ) ;
#6633 = CARTESIAN_POINT ( 'NONE',  ( 5.250000000000000000, -28.81249999931720396, -6.429395695523604153E-16 ) ) ;
#6634 = CARTESIAN_POINT ( 'NONE',  ( -2.108492589042352261, -4.750659073900640017, 2.134148098076933397 ) ) ;
#6635 = CARTESIAN_POINT ( 'NONE',  ( -5.249999999999999112, -27.45833333265053611, -3.031088913245534755 ) ) ;
#6636 = CARTESIAN_POINT ( 'NONE',  ( -5.249999999999999112, -27.66666666598386826, 3.031088913245538308 ) ) ;
#6637 = DIRECTION ( 'NONE',  ( 0.000000000000000000, -1.000000000000000000, 0.000000000000000000 ) ) ;
#6638 = CARTESIAN_POINT ( 'NONE',  ( 1.431606283892619347, -0.7493409260993610932, 3.507514324621464397 ) ) ;
#6639 = FACE_BOUND ( 'NONE', #4349, .T. ) ;
#6640 = CARTESIAN_POINT ( 'NONE',  ( 2.625000000000000444, -27.70833333333333215, -4.546633369868303021 ) ) ;
#6641 = COLOUR_RGB ( '',0.8941176470588234615, 0.8941176470588234615, 0.8941176470588234615 ) ;
#6642 = CARTESIAN_POINT ( 'NONE',  ( 1.142306659890740623E-15, -28.01562499965860553, 6.218427825808274356 ) ) ;
#6643 = CARTESIAN_POINT ( 'NONE',  ( -0.01814118441321889430, -5.449340926099361937, 4.000000000000000000 ) ) ;
#6644 = CYLINDRICAL_SURFACE ( 'NONE', #2508, 5.250000000000000000 ) ;
#6645 = EDGE_LOOP ( 'NONE', ( #4466, #8198 ) ) ;
#6646 = CARTESIAN_POINT ( 'NONE',  ( -2.692658234374996518, -29.03645833299193413, 4.663820869356208654 ) ) ;
#6647 = CARTESIAN_POINT ( 'NONE',  ( -2.134148098076932953, -4.350659073900638774, -2.108492589042352705 ) ) ;
#6648 = ORIENTED_EDGE ( 'NONE', *, *, #698, .T. ) ;
#6649 = CARTESIAN_POINT ( 'NONE',  ( -1.113604000661152470E-15, -27.56250000000000000, 6.062177826491070398 ) ) ;
#6650 = AXIS2_PLACEMENT_3D ( 'NONE', #6328, #1541, #5910 ) ;
#6651 = CARTESIAN_POINT ( 'NONE',  ( -1.431606283892693066, -3.250659073900639129, 3.507514324621434199 ) ) ;
#6652 = CARTESIAN_POINT ( 'NONE',  ( 5.250000000000000888, -27.64583333333333570, 3.031088913245532979 ) ) ;
#6653 = PRODUCT_DEFINITION ( 'UNKNOWN', '', #4998, #306 ) ;
#6654 = CARTESIAN_POINT ( 'NONE',  ( 2.557341765624996821, -29.15104166700806587, 4.429445870380401828 ) ) ;
#6655 = CARTESIAN_POINT ( 'NONE',  ( 1.467888652719048226, -2.949340926099361493, -3.492485675378536047 ) ) ;
#6656 = FACE_OUTER_BOUND ( 'NONE', #5224, .T. ) ;
#6657 = CARTESIAN_POINT ( 'NONE',  ( 9.180150650966086169E-15, -28.81250000000000000, 5.250000000000000000 ) ) ;
#6658 = CARTESIAN_POINT ( 'NONE',  ( 3.616337804771879580E-16, -28.60937500034139802, -5.905927827173866440 ) ) ;
#6659 = CARTESIAN_POINT ( 'NONE',  ( 2.033577675846918216E-14, -27.06250000000000355, 5.250000000000000888 ) ) ;
#6660 = ORIENTED_EDGE ( 'NONE', *, *, #2365, .T. ) ;
#6661 = DIRECTION ( 'NONE',  ( 0.000000000000000000, -0.000000000000000000, 1.000000000000000000 ) ) ;
#6662 = CARTESIAN_POINT ( 'NONE',  ( 5.114683531249998971, -28.13020833367473017, 2.952963913586936329 ) ) ;
#6663 = AXIS2_PLACEMENT_3D ( 'NONE', #1760, #7434, #2460 ) ;
#6664 = EDGE_LOOP ( 'NONE', ( #8316, #475 ) ) ;
#6665 = CARTESIAN_POINT ( 'NONE',  ( 1.975475456537005874E-15, -27.93749999999999289, 5.250000000000000000 ) ) ;
#6666 = EDGE_CURVE ( 'NONE', #8226, #7186, #2360, .T. ) ;
#6667 = CARTESIAN_POINT ( 'NONE',  ( -2.692658234374996518, -27.56770833299193413, 4.663820869356208654 ) ) ;
#6668 = CARTESIAN_POINT ( 'NONE',  ( 3.992485675378568910, -5.450659073900638418, -1.674995433905514863 ) ) ;
#6669 = CARTESIAN_POINT ( 'NONE',  ( 5.385316468749999252, -28.46354166632526628, -3.109213912904139399 ) ) ;
#6670 = PRESENTATION_LAYER_ASSIGNMENT (  '', '', ( #3419 ) ) ;
#6671 = ORIENTED_EDGE ( 'NONE', *, *, #4478, .T. ) ;
#6672 = EDGE_CURVE ( 'NONE', #2870, #5029, #2637, .T. ) ;
#6673 = CARTESIAN_POINT ( 'NONE',  ( 1.045839947578414884E-14, -27.99999999931720041, -5.250000000000000000 ) ) ;
#6674 = CARTESIAN_POINT ( 'NONE',  ( 2.625000000000000444, -29.73958333401613174, -4.546633369868303021 ) ) ;
#6675 = CARTESIAN_POINT ( 'NONE',  ( 2.692658234375002735, -27.77604166632526628, 4.663820869356205101 ) ) ;
#6676 = AXIS2_PLACEMENT_3D ( 'NONE', #4387, #7409, #1032 ) ;
#6677 = ORIENTED_EDGE ( 'NONE', *, *, #3723, .F. ) ;
#6678 = CARTESIAN_POINT ( 'NONE',  ( 1.406733260263403507, -28.76116454900182973, -5.249999999999994671 ) ) ;
#6679 = EDGE_CURVE ( 'NONE', #874, #7322, #9181, .T. ) ;
#6680 = CARTESIAN_POINT ( 'NONE',  ( -2.134148098076932953, -1.150659073900639040, -2.108492589042352705 ) ) ;
#6681 = CARTESIAN_POINT ( 'NONE',  ( -5.249999999999999112, -28.41666666598387181, 3.031088913245538308 ) ) ;
#6682 = CARTESIAN_POINT ( 'NONE',  ( 2.487701488670255756, -2.849340926099361404, -2.462045979635577364 ) ) ;
#6683 =( BOUNDED_CURVE ( )  B_SPLINE_CURVE ( 2, ( #3789, #8614, #3050, #2337, #8662, #5168, #2245, #4480, #5118 ),
 .UNSPECIFIED., .F., .F. ) 
 B_SPLINE_CURVE_WITH_KNOTS ( ( 3, 2, 2, 2, 3 ),
 ( 0.8958333333333333703, 0.9027777777777777901, 0.9166666666666666297, 0.9305555555555555802, 0.9375000002123526910 ),
 .UNSPECIFIED. ) 
 CURVE ( )  GEOMETRIC_REPRESENTATION_ITEM ( )  RATIONAL_B_SPLINE_CURVE ( ( 0.9330127018922192983, 0.9330127018922198534, 1.000000000000000000, 0.8660254037844387076, 1.000000000000000000, 0.8660254037844387076, 1.000000000000000000, 0.9330126998438290631, 0.9330127018922194093 ) ) 
 REPRESENTATION_ITEM ( '' )  );
#6684 = CARTESIAN_POINT ( 'NONE',  ( 5.249999999999999112, -29.04166666598387181, -3.031088913245536975 ) ) ;
#6685 = DIRECTION ( 'NONE',  ( 1.000000000000000000, 0.000000000000000000, 0.000000000000000000 ) ) ;
#6686 = CARTESIAN_POINT ( 'NONE',  ( 0.000000000000000000, 0.000000000000000000, 0.000000000000000000 ) ) ;
#6687 = CARTESIAN_POINT ( 'NONE',  ( 5.385316468750001029, -28.47395833299193413, 3.109213912904135846 ) ) ;
#6688 = CARTESIAN_POINT ( 'NONE',  ( 2.815599370228847320, -4.049340926099360694, 2.841254879263533262 ) ) ;
#6689 = CARTESIAN_POINT ( 'NONE',  ( 6.429395695523604153E-16, -27.00000000000000000, 5.250000000000000000 ) ) ;
#6690 = ORIENTED_EDGE ( 'NONE', *, *, #672, .F. ) ;
#6691 = CARTESIAN_POINT ( 'NONE',  ( -5.385316468749998364, -27.80729166632526628, 3.109213912904140287 ) ) ;
#6692 = CARTESIAN_POINT ( 'NONE',  ( -3.507514324621434199, -6.050659073900638951, -1.431606283892695064 ) ) ;
#6693 = COLOUR_RGB ( '',0.8941176470588234615, 0.8941176470588234615, 0.8941176470588234615 ) ;
#6694 = ORIENTED_EDGE ( 'NONE', *, *, #2154, .T. ) ;
#6695 = CARTESIAN_POINT ( 'NONE',  ( -2.624999999999998668, -28.41666666666666785, -4.546633369868303021 ) ) ;
#6696 = EDGE_CURVE ( 'NONE', #5282, #3224, #6504, .T. ) ;
#6697 = CARTESIAN_POINT ( 'NONE',  ( -2.557341765624999042, -27.08854166700806232, -4.429445870380400052 ) ) ;
#6698 = VERTEX_POINT ( 'NONE', #4073 ) ;
#6699 = SHAPE_REPRESENTATION_RELATIONSHIP ( 'NONE' , 'NONE' ,  #4384, #4954 ) ;
#6700 = CARTESIAN_POINT ( 'NONE',  ( -1.406733260263395735, -29.35491455036742892, 5.250000000000000000 ) ) ;
#6701 = EDGE_LOOP ( 'NONE', ( #1580, #8515, #415, #5711 ) ) ;
#6702 = CARTESIAN_POINT ( 'NONE',  ( 5.114683531249998971, -28.88020833367473017, 2.952963913586936329 ) ) ;
#6703 = CARTESIAN_POINT ( 'NONE',  ( 2.462045979635577364, -2.449340926099361049, 2.487701488670255312 ) ) ;
#6704 = CARTESIAN_POINT ( 'NONE',  ( 3.367778697655221012E-16, -9.999999999999998224, -2.750000000000000000 ) ) ;
#6705 = DIRECTION ( 'NONE',  ( 0.000000000000000000, 1.000000000000000000, 0.000000000000000000 ) ) ;
#6706 = CARTESIAN_POINT ( 'NONE',  ( -1.084901341431563923E-15, -28.48437500034139802, 5.905927827173866440 ) ) ;
#6707 = EDGE_CURVE ( 'NONE', #8870, #7281, #4248, .T. ) ;
#6708 = CARTESIAN_POINT ( 'NONE',  ( 2.300847884672513123E-14, -27.46875000068279604, -5.250000000000000000 ) ) ;
#6709 = CARTESIAN_POINT ( 'NONE',  ( 0.000000000000000000, -30.00000000000000000, 5.250000000000000000 ) ) ;
#6710 = ORIENTED_EDGE ( 'NONE', *, *, #9006, .F. ) ;
#6711 = PLANE ( 'NONE',  #5320 ) ;
#6712 = CARTESIAN_POINT ( 'NONE',  ( 1.142306659890740623E-15, -29.29687499965859487, 6.218427825808274356 ) ) ;
#6713 = CARTESIAN_POINT ( 'NONE',  ( 2.841254879263533262, -1.249340926099360871, -2.815599370228847320 ) ) ;
#6714 = CARTESIAN_POINT ( 'NONE',  ( 5.385316468750001029, -29.00520833299193413, 3.109213912904135846 ) ) ;
#6715 = VERTEX_POINT ( 'NONE', #9127 ) ;
#6716 = DIRECTION ( 'NONE',  ( 0.000000000000000000, 0.000000000000000000, -1.000000000000000000 ) ) ;
#6717 = CARTESIAN_POINT ( 'NONE',  ( 5.249999999999999112, -28.55208333401613174, 3.031088913245538308 ) ) ;
#6718 = CARTESIAN_POINT ( 'NONE',  ( 1.142306659890740623E-15, -27.29687499965859843, 6.218427825808274356 ) ) ;
#6719 = PRODUCT_DEFINITION_CONTEXT ( 'detailed design', #9134, 'design' ) ;
#6720 = VECTOR ( 'NONE', #1929, 1000.000000000000000 ) ;
#6721 = ORIENTED_EDGE ( 'NONE', *, *, #3064, .F. ) ;
#6722 = CARTESIAN_POINT ( 'NONE',  ( 2.692658234375002735, -27.99479166632526628, 4.663820869356205101 ) ) ;
#6723 = CARTESIAN_POINT ( 'NONE',  ( -3.007514324621435531, -2.850659073900640106, -1.224499502706142273 ) ) ;
#6724 = CARTESIAN_POINT ( 'NONE',  ( 0.000000000000000000, 75.00000000000000000, 0.000000000000000000 ) ) ;
#6725 = EDGE_CURVE ( 'NONE', #8837, #3172, #8940, .T. ) ;
#6726 = VECTOR ( 'NONE', #3619, 1000.000000000000000 ) ;
#6727 = VECTOR ( 'NONE', #6943, 1000.000000000000000 ) ;
#6728 = CARTESIAN_POINT ( 'NONE',  ( 2.624999999999998668, -28.02083333265053255, -4.546633369868303021 ) ) ;
#6729 = CARTESIAN_POINT ( 'NONE',  ( 1.185285273922203525E-14, -28.71875000068279959, -5.249999999999999112 ) ) ;
#6730 = CARTESIAN_POINT ( 'NONE',  ( -1.431606283892620235, -1.549340926099361138, -3.507514324621463953 ) ) ;
#6731 = CARTESIAN_POINT ( 'NONE',  ( -5.114683531249999859, -29.50520833367473017, -2.952963913586935440 ) ) ;
#6732 = ORIENTED_EDGE ( 'NONE', *, *, #5568, .F. ) ;
#6733 = DIRECTION ( 'NONE',  ( 0.000000000000000000, 0.000000000000000000, 1.000000000000000000 ) ) ;
#6734 = CARTESIAN_POINT ( 'NONE',  ( -2.692658234374996518, -29.03645833299193413, 4.663820869356208654 ) ) ;
#6735 = CARTESIAN_POINT ( 'NONE',  ( -4.007514324621467949, -1.949340926099360827, 1.638713065079161924 ) ) ;
#6736 = AXIS2_PLACEMENT_3D ( 'NONE', #4548, #5237, #7196 ) ;
#6737 = DIRECTION ( 'NONE',  ( 0.000000000000000000, -1.000000000000000000, 0.000000000000000000 ) ) ;
#6738 = ORIENTED_EDGE ( 'NONE', *, *, #7992, .T. ) ;
#6739 = CARTESIAN_POINT ( 'NONE',  ( 5.385316468750001029, -27.97395833299193413, 3.109213912904135846 ) ) ;
#6740 = ADVANCED_FACE ( 'NONE', ( #134 ), #3550, .F. ) ;
#6741 = CARTESIAN_POINT ( 'NONE',  ( -3.492485675378566246, -4.650659073900639484, 1.467888652718973397 ) ) ;
#6742 = VERTEX_POINT ( 'NONE', #4890 ) ;
#6743 = CARTESIAN_POINT ( 'NONE',  ( -2.624999999999998668, -28.16666666666666785, -4.546633369868303021 ) ) ;
#6744 = PRODUCT_DEFINITION_SHAPE ( 'NONE', 'NONE',  #9197 ) ;
#6745 = CARTESIAN_POINT ( 'NONE',  ( -3.507514324621433754, -7.650659073900639484, -1.431606283892695064 ) ) ;
#6746 =( BOUNDED_CURVE ( )  B_SPLINE_CURVE ( 2, ( #3058, #1599, #7226, #4352, #5879, #8716, #3799, #6576, #8625 ),
 .UNSPECIFIED., .F., .F. ) 
 B_SPLINE_CURVE_WITH_KNOTS ( ( 3, 2, 2, 2, 3 ),
 ( 0.8958333333333333703, 0.9027777777777777901, 0.9166666666666666297, 0.9305555555555555802, 0.9375000000000000000 ),
 .UNSPECIFIED. ) 
 CURVE ( )  GEOMETRIC_REPRESENTATION_ITEM ( )  RATIONAL_B_SPLINE_CURVE ( ( 0.9330127018922192983, 0.9330127018922198534, 1.000000000000000000, 0.8660254037844387076, 1.000000000000000000, 0.8660254037844387076, 1.000000000000000000, 0.9330127018922194093, 0.9330127018922194093 ) ) 
 REPRESENTATION_ITEM ( '' )  );
#6747 = CARTESIAN_POINT ( 'NONE',  ( -0.01814118441313947866, -2.550659073900638951, -3.500000000000000000 ) ) ;
#6748 = ORIENTED_EDGE ( 'NONE', *, *, #7785, .T. ) ;
#6749 = SURFACE_STYLE_USAGE ( .BOTH. , #2432 ) ;
#6750 = CARTESIAN_POINT ( 'NONE',  ( 2.624999999999998668, -27.08333333333333570, -4.546633369868303021 ) ) ;
#6751 = ADVANCED_FACE ( 'NONE', ( #5550 ), #5509, .F. ) ;
#6752 = ORIENTED_EDGE ( 'NONE', *, *, #5454, .T. ) ;
#6753 = CARTESIAN_POINT ( 'NONE',  ( 5.114683531250000748, -28.35937500034139447, 0.000000000000000000 ) ) ;
#6754 = CARTESIAN_POINT ( 'NONE',  ( -1.431606283892620235, -7.949340926099361049, -3.507514324621463953 ) ) ;
#6755 = CARTESIAN_POINT ( 'NONE',  ( 1.185285273922203525E-14, -28.93749999999999645, -5.249999999999999112 ) ) ;
#6756 = DIRECTION ( 'NONE',  ( 0.000000000000000000, -1.000000000000000000, 0.000000000000000000 ) ) ;
#6757 = CARTESIAN_POINT ( 'NONE',  ( 2.557341765625000818, -28.88020833367473017, -4.429445870380400052 ) ) ;
#6758 = CARTESIAN_POINT ( 'NONE',  ( 0.000000000000000000, -30.00000000000000000, 0.000000000000000000 ) ) ;
#6759 = CARTESIAN_POINT ( 'NONE',  ( 4.898587196589412829E-16, 74.00000000000001421, 4.000000000000000000 ) ) ;
#6760 = CARTESIAN_POINT ( 'NONE',  ( -5.114683531250000748, -27.21354166700806587, 2.952963913586931888 ) ) ;
#6761 = ORIENTED_EDGE ( 'NONE', *, *, #2985, .T. ) ;
#6762 = DIRECTION ( 'NONE',  ( 0.000000000000000000, 1.000000000000000000, 0.000000000000000000 ) ) ;
#6763 = CARTESIAN_POINT ( 'NONE',  ( 5.385316468749999252, -29.21354166632527338, -3.109213912904138954 ) ) ;
#6764 = CARTESIAN_POINT ( 'NONE',  ( -5.250000000000000888, -28.60416666666666430, 3.031088913245533423 ) ) ;
#6765 = CARTESIAN_POINT ( 'NONE',  ( 0.000000000000000000, -53.00000000000000000, 1.749999999999999778 ) ) ;
#6766 = CARTESIAN_POINT ( 'NONE',  ( -5.385316468750000141, -29.85937499965859843, 0.000000000000000000 ) ) ;
#6767 = CARTESIAN_POINT ( 'NONE',  ( 0.01814118441313467001, -6.550659073900640728, 4.000000000000000000 ) ) ;
#6768 = VERTEX_POINT ( 'NONE', #6251 ) ;
#6769 = DIRECTION ( 'NONE',  ( 0.000000000000000000, -1.000000000000000000, 0.000000000000000000 ) ) ;
#6770 = CARTESIAN_POINT ( 'NONE',  ( 5.250000000000000000, -28.03125000068279604, 0.000000000000000000 ) ) ;
#6771 = EDGE_CURVE ( 'NONE', #8099, #4014, #3375, .T. ) ;
#6772 = CARTESIAN_POINT ( 'NONE',  ( 2.692658234374998738, -29.44270833299193413, -4.663820869356206877 ) ) ;
#6773 = ORIENTED_EDGE ( 'NONE', *, *, #4774, .F. ) ;
#6774 = CARTESIAN_POINT ( 'NONE',  ( -2.692658234374996518, -28.78645833299193413, 4.663820869356208654 ) ) ;
#6775 = CARTESIAN_POINT ( 'NONE',  ( -0.01814118441313947866, -0.9506590739006390844, -3.500000000000000000 ) ) ;
#6776 = PRODUCT_RELATED_PRODUCT_CATEGORY ( 'part', '', ( #1433 ) ) ;
#6777 = CARTESIAN_POINT ( 'NONE',  ( -1.975475456537005874E-15, -29.56250000000000000, 5.250000000000000000 ) ) ;
#6778 =( NAMED_UNIT ( * ) PLANE_ANGLE_UNIT ( ) SI_UNIT ( $, .RADIAN. ) );
#6779 = CARTESIAN_POINT ( 'NONE',  ( 5.249999999999999112, -28.22916666666666430, -3.031088913245534755 ) ) ;
#6780 = CARTESIAN_POINT ( 'NONE',  ( 2.033577675846918216E-14, -27.84375000068279959, 5.250000000000000888 ) ) ;
#6781 = LINE ( 'NONE', #3255, #4216 ) ;
#6782 = CARTESIAN_POINT ( 'NONE',  ( 5.250000000000000000, -27.75000000000000000, 0.000000000000000000 ) ) ;
#6783 = ITEM_DEFINED_TRANSFORMATION ( 'NONE', 'NONE', #264,  #888 ) ;
#6784 = CARTESIAN_POINT ( 'NONE',  ( 2.692658234375002735, -29.99479166632526628, 4.663820869356205101 ) ) ;
#6785 = CARTESIAN_POINT ( 'NONE',  ( -1.467888652719046449, -3.749340926099360871, 3.492485675378536047 ) ) ;
#6786 = CARTESIAN_POINT ( 'NONE',  ( -9.180150650966086169E-15, -28.62499999931720396, 5.249999999999999112 ) ) ;
#6787 = CARTESIAN_POINT ( 'NONE',  ( -2.692658234374996518, -28.03645833299193413, 4.663820869356208654 ) ) ;
#6788 = CARTESIAN_POINT ( 'NONE',  ( 3.500000000000000000, -6.950659073900639306, -0.01814118441313969030 ) ) ;
#6789 = EDGE_CURVE ( 'NONE', #2434, #8455, #8999, .T. ) ;
#6790 = EDGE_LOOP ( 'NONE', ( #7502, #1101 ) ) ;
#6791 = DIRECTION ( 'NONE',  ( -0.000000000000000000, -1.000000000000000000, -0.000000000000000000 ) ) ;
#6792 = CARTESIAN_POINT ( 'NONE',  ( 1.000000000000000000, -20.00000000000000000, -1.118033988749894680 ) ) ;
#6793 = EDGE_CURVE ( 'NONE', #7910, #4963, #5106, .T. ) ;
#6794 = CARTESIAN_POINT ( 'NONE',  ( 1.467888652718972731, -1.850659073900638996, 3.492485675378566246 ) ) ;
#6795 = ORIENTED_EDGE ( 'NONE', *, *, #6392, .F. ) ;
#6796 =( LENGTH_UNIT ( ) NAMED_UNIT ( * ) SI_UNIT ( .MILLI., .METRE. ) );
#6797 = CARTESIAN_POINT ( 'NONE',  ( 2.624999999999998668, -27.83333333333333215, -4.546633369868303021 ) ) ;
#6798 = ORIENTED_EDGE ( 'NONE', *, *, #2154, .F. ) ;
#6799 = EDGE_CURVE ( 'NONE', #6343, #451, #4847, .T. ) ;
#6800 = CARTESIAN_POINT ( 'NONE',  ( 5.114683531250000748, -28.83854166700806587, -2.952963913586932776 ) ) ;
#6801 = CARTESIAN_POINT ( 'NONE',  ( -2.462045979635576920, -8.049340926099361582, -2.487701488670255756 ) ) ;
#6802 = CARTESIAN_POINT ( 'NONE',  ( -2.625000000000002220, -28.08333333333333215, 4.546633369868302132 ) ) ;
#6803 = CARTESIAN_POINT ( 'NONE',  ( 3.616337804771879580E-16, -28.35937500034139447, -5.905927827173866440 ) ) ;
#6804 = MECHANICAL_DESIGN_GEOMETRIC_PRESENTATION_REPRESENTATION (  '', ( #7692 ), #409 ) ;
#6805 = CARTESIAN_POINT ( 'NONE',  ( -5.250000000000000000, -29.18749999931720396, 0.000000000000000000 ) ) ;
#6806 = DIRECTION ( 'NONE',  ( 0.000000000000000000, -1.000000000000000000, 0.000000000000000000 ) ) ;
#6807 = LINE ( 'NONE', #6709, #2235 ) ;
#6808 = CARTESIAN_POINT ( 'NONE',  ( 1.406733260263402174, -27.05133545031536713, 5.249999999999995559 ) ) ;
#6809 = CARTESIAN_POINT ( 'NONE',  ( 0.01814118441320878086, -3.049340926099361138, -3.000000000000000444 ) ) ;
#6810 = CARTESIAN_POINT ( 'NONE',  ( -2.557341765624999042, -28.58854166700806587, -4.429445870380400052 ) ) ;
#6811 = ORIENTED_EDGE ( 'NONE', *, *, #2985, .F. ) ;
#6812 = FACE_OUTER_BOUND ( 'NONE', #66, .T. ) ;
#6813 = CARTESIAN_POINT ( 'NONE',  ( 1.142306659890740623E-15, -28.79687499965860198, 6.218427825808274356 ) ) ;
#6814 = CARTESIAN_POINT ( 'NONE',  ( -2.624999999999998668, -28.66666666666666785, -4.546633369868303021 ) ) ;
#6815 = DIRECTION ( 'NONE',  ( 0.000000000000000000, 1.000000000000000000, 0.000000000000000000 ) ) ;
#6816 = CARTESIAN_POINT ( 'NONE',  ( -2.692658234375000514, -29.65104166632526983, -4.663820869356205989 ) ) ;
#6817 = CARTESIAN_POINT ( 'NONE',  ( -4.007514324621467949, -6.749340926099361759, 1.638713065079161924 ) ) ;
#6818 = ORIENTED_EDGE ( 'NONE', *, *, #7770, .T. ) ;
#6819 = AXIS2_PLACEMENT_3D ( 'NONE', #2705, #464, #4696 ) ;
#6820 = CARTESIAN_POINT ( 'NONE',  ( 5.249999999999999112, -29.26041666734946389, -3.031088913245534755 ) ) ;
#6821 = CARTESIAN_POINT ( 'NONE',  ( -5.250000000000000000, -28.40625000068279604, -6.429395695523604153E-16 ) ) ;
#6822 = ADVANCED_FACE ( 'NONE', ( #7653 ), #1276, .F. ) ;
#6823 = CARTESIAN_POINT ( 'NONE',  ( -5.385316468749998364, -29.08854166632526628, 3.109213912904140287 ) ) ;
#6824 = EDGE_CURVE ( 'NONE', #1880, #6258, #8643, .T. ) ;
#6825 = VERTEX_POINT ( 'NONE', #5250 ) ;
#6826 = AXIS2_PLACEMENT_3D ( 'NONE', #5193, #8035, #8638 ) ;
#6827 = CARTESIAN_POINT ( 'NONE',  ( 2.692658234374998738, -28.91145833299193413, -4.663820869356206877 ) ) ;
#6828 = CARTESIAN_POINT ( 'NONE',  ( 3.492485675378566690, -2.250659073900639573, -1.467888652718972287 ) ) ;
#6829 = CARTESIAN_POINT ( 'NONE',  ( 1.406733260263394625, -29.44866454968462932, -5.250000000000000000 ) ) ;
#6830 =( BOUNDED_CURVE ( )  B_SPLINE_CURVE ( 2, ( #245, #1596, #7365, #5829, #3097, #1503, #6570, #293, #5875 ),
 .UNSPECIFIED., .F., .T. ) 
 B_SPLINE_CURVE_WITH_KNOTS ( ( 3, 2, 2, 2, 3 ),
 ( 0.1875000000000000000, 0.1944444444444444475, 0.2083333333333333426, 0.2222222222222222099, 0.2291666666666666574 ),
 .UNSPECIFIED. ) 
 CURVE ( )  GEOMETRIC_REPRESENTATION_ITEM ( )  RATIONAL_B_SPLINE_CURVE ( ( 0.9330127018922194093, 0.9330127018922194093, 1.000000000000000000, 0.8660254037844387076, 1.000000000000000000, 0.8660254037844387076, 1.000000000000000000, 0.9330127018922194093, 0.9330127018922194093 ) ) 
 REPRESENTATION_ITEM ( '' )  );
#6831 = CARTESIAN_POINT ( 'NONE',  ( 1.185285273922203525E-14, -28.93749999999999645, -5.250000000000000000 ) ) ;
#6832 = CIRCLE ( 'NONE', #5782, 4.000000000000000000 ) ;
#6833 = CARTESIAN_POINT ( 'NONE',  ( 2.324088772396477476E-15, -27.31250000000000000, -5.250000000000000000 ) ) ;
#6834 = CARTESIAN_POINT ( 'NONE',  ( -5.114683531250000748, -29.48437500034139802, -6.263680815196995234E-16 ) ) ;
#6835 = ORIENTED_EDGE ( 'NONE', *, *, #7462, .T. ) ;
#6836 = CIRCLE ( 'NONE', #2833, 5.250000000000000000 ) ;
#6837 = PRODUCT_CONTEXT ( 'NONE', #1268, 'mechanical' ) ;
#6838 = CARTESIAN_POINT ( 'NONE',  ( -3.807688866302469071E-16, -29.64062499965859843, -6.218427825808274356 ) ) ;
#6839 = CARTESIAN_POINT ( 'NONE',  ( 2.134148098076978251, -1.249340926099361537, -2.108492589042307408 ) ) ;
#6840 = LINE ( 'NONE', #4053, #7709 ) ;
#6841 = CARTESIAN_POINT ( 'NONE',  ( -5.385316468749998364, -28.55729166632527338, 3.109213912904140287 ) ) ;
#6842 = CARTESIAN_POINT ( 'NONE',  ( 3.500000000000000000, -2.150659073900639040, -0.01814118441313969030 ) ) ;
#6843 = VERTEX_POINT ( 'NONE', #878 ) ;
#6844 = CARTESIAN_POINT ( 'NONE',  ( 2.625000000000002220, -30.10416666598386826, 4.546633369868302132 ) ) ;
#6845 = PRODUCT_DEFINITION_CONTEXT ( 'detailed design', #43, 'design' ) ;
#6846 = VECTOR ( 'NONE', #8597, 1000.000000000000000 ) ;
#6847 = DIRECTION ( 'NONE',  ( 0.000000000000000000, 0.000000000000000000, 1.000000000000000000 ) ) ;
#6848 = CARTESIAN_POINT ( 'NONE',  ( 2.462045979635629767, -2.350659073900639218, -2.487701488670203354 ) ) ;
#6849 = VERTEX_POINT ( 'NONE', #3866 ) ;
#6850 = CARTESIAN_POINT ( 'NONE',  ( 5.250000000000000000, -29.12499999999999645, -6.429395695523604153E-16 ) ) ;
#6851 = COLOUR_RGB ( '',0.8941176470588234615, 0.8941176470588234615, 0.8941176470588234615 ) ;
#6852 = VERTEX_POINT ( 'NONE', #7252 ) ;
#6853 = CARTESIAN_POINT ( 'NONE',  ( -5.114683531250000748, -28.73437500034139802, -6.263680815196995234E-16 ) ) ;
#6854 = CARTESIAN_POINT ( 'NONE',  ( 3.492485675378536047, -7.349340926099362292, 1.467888652719046672 ) ) ;
#6855 = CARTESIAN_POINT ( 'NONE',  ( -1.000000000000000000, -29.00000000000000355, 1.118033988749894680 ) ) ;
#6856 = CARTESIAN_POINT ( 'NONE',  ( 5.250000000000000000, -30.00000000000000000, 0.000000000000000000 ) ) ;
#6857 = DIRECTION ( 'NONE',  ( 0.000000000000000000, -1.000000000000000000, 0.000000000000000000 ) ) ;
#6858 = ADVANCED_FACE ( 'NONE', ( #7395 ), #6644, .F. ) ;
#6859 = CARTESIAN_POINT ( 'NONE',  ( -1.943399160878812371, -1.460316824068199838E-13, 2.858293051873583845 ) ) ;
#6860 = CARTESIAN_POINT ( 'NONE',  ( -1.084901341431563923E-15, -26.92187500034139802, 5.905927827173866440 ) ) ;
#6861 = DIRECTION ( 'NONE',  ( 1.000000000000000000, 0.000000000000000000, 0.000000000000000000 ) ) ;
#6862 = CARTESIAN_POINT ( 'NONE',  ( 2.557341765624996821, -29.21354166700806587, 4.429445870380401828 ) ) ;
#6863 = DIRECTION ( 'NONE',  ( 0.000000000000000000, -1.000000000000000000, 0.000000000000000000 ) ) ;
#6864 = CARTESIAN_POINT ( 'NONE',  ( -5.385316468750001029, -28.38020833299193413, -3.109213912904136734 ) ) ;
#6865 = CARTESIAN_POINT ( 'NONE',  ( -5.250000000000000888, -29.13541666734946389, 3.031088913245533423 ) ) ;
#6866 = DIRECTION ( 'NONE',  ( 0.000000000000000000, 1.000000000000000000, 0.000000000000000000 ) ) ;
#6867 = CARTESIAN_POINT ( 'NONE',  ( 2.692658234375002735, -30.02604166632526983, 4.663820869356205101 ) ) ;
#6868 = CARTESIAN_POINT ( 'NONE',  ( 2.462045979635577364, -0.8493409260993610710, 2.487701488670255312 ) ) ;
#6869 = CARTESIAN_POINT ( 'NONE',  ( -0.01814118441321365544, -2.249340926099361315, 3.500000000000000000 ) ) ;
#6870 = VERTEX_POINT ( 'NONE', #2420 ) ;
#6871 = DIRECTION ( 'NONE',  ( 0.000000000000000000, 0.000000000000000000, 1.000000000000000000 ) ) ;
#6872 = CARTESIAN_POINT ( 'NONE',  ( -5.250000000000000000, -28.42708333401612819, -3.031088913245536531 ) ) ;
#6873 = CARTESIAN_POINT ( 'NONE',  ( -3.807688866302469071E-16, -29.67187499965860198, -6.218427825808274356 ) ) ;
#6874 = VERTEX_POINT ( 'NONE', #1070 ) ;
#6875 = CARTESIAN_POINT ( 'NONE',  ( 2.692658234375002735, -28.49479166632526628, 4.663820869356205101 ) ) ;
#6876 = CARTESIAN_POINT ( 'NONE',  ( 0.01814118441313990887, -3.350659073900639218, 3.500000000000000000 ) ) ;
#6877 = CARTESIAN_POINT ( 'NONE',  ( 5.250000000000000000, -29.78125000068279604, 0.000000000000000000 ) ) ;
#6878 = EDGE_CURVE ( 'NONE', #2431, #8870, #182, .T. ) ;
#6879 = CARTESIAN_POINT ( 'NONE',  ( -5.250000000000000000, -28.43749999931720396, 0.000000000000000000 ) ) ;
#6880 = CARTESIAN_POINT ( 'NONE',  ( 2.161402558328724325E-14, -28.81250000000000355, -5.250000000000000000 ) ) ;
#6881 = VECTOR ( 'NONE', #8983, 1000.000000000000000 ) ;
#6882 = CARTESIAN_POINT ( 'NONE',  ( 0.000000000000000000, -9.999999999999998224, 0.000000000000000000 ) ) ;
#6883 = CARTESIAN_POINT ( 'NONE',  ( 4.898587196589412829E-16, 79.00000000000001421, 4.000000000000000000 ) ) ;
#6884 = CONTEXT_DEPENDENT_SHAPE_REPRESENTATION ( #3548, #8165 ) ;
#6885 = CARTESIAN_POINT ( 'NONE',  ( 5.385316468750000141, -29.20312499965859843, -6.595110575850215044E-16 ) ) ;
#6886 = CARTESIAN_POINT ( 'NONE',  ( 2.487701488670255756, -4.449340926099361937, -2.462045979635577364 ) ) ;
#6887 = CARTESIAN_POINT ( 'NONE',  ( -2.625000000000000444, -29.54166666666666785, -4.546633369868303021 ) ) ;
#6888 = CIRCLE ( 'NONE', #8663, 5.250000000000000000 ) ;
#6889 = CARTESIAN_POINT ( 'NONE',  ( -5.385316468750000141, -29.82812499965859843, 0.000000000000000000 ) ) ;
#6890 = CARTESIAN_POINT ( 'NONE',  ( 3.507514324621434199, -6.850659073900638774, 1.431606283892693066 ) ) ;
#6891 = MECHANICAL_DESIGN_GEOMETRIC_PRESENTATION_REPRESENTATION (  '', ( #5984 ), #501 ) ;
#6892 = ORIENTED_EDGE ( 'NONE', *, *, #1508, .T. ) ;
#6893 = DIRECTION ( 'NONE',  ( 0.000000000000000000, 1.000000000000000000, 0.000000000000000000 ) ) ;
#6894 = DIRECTION ( 'NONE',  ( -0.8660254037844402619, 0.4999999999999970579, -0.000000000000000000 ) ) ;
#6895 = CARTESIAN_POINT ( 'NONE',  ( 3.507514324621434199, -5.250659073900640905, 1.431606283892693066 ) ) ;
#6896 = EDGE_CURVE ( 'NONE', #7225, #8711, #387, .T. ) ;
#6897 = AXIS2_PLACEMENT_3D ( 'NONE', #4783, #8186, #2464 ) ;
#6898 = ORIENTED_EDGE ( 'NONE', *, *, #3839, .T. ) ;
#6899 =( NAMED_UNIT ( * ) SI_UNIT ( $, .STERADIAN. ) SOLID_ANGLE_UNIT ( ) );
#6900 = CARTESIAN_POINT ( 'NONE',  ( 1.113604000661152470E-15, -28.43750000000000355, 6.062177826491070398 ) ) ;
#6901 = ORIENTED_EDGE ( 'NONE', *, *, #7017, .F. ) ;
#6902 = CARTESIAN_POINT ( 'NONE',  ( 5.114683531249998971, -27.63020833367473017, 2.952963913586936329 ) ) ;
#6903 = CARTESIAN_POINT ( 'NONE',  ( -3.007514324621463508, -5.149340926099361226, 1.224499502706077658 ) ) ;
#6904 = DIRECTION ( 'NONE',  ( 0.000000000000000000, 1.000000000000000000, 0.000000000000000000 ) ) ;
#6905 = CARTESIAN_POINT ( 'NONE',  ( -5.114683531249999859, -27.56770833367473017, -2.952963913586935440 ) ) ;
#6906 = CARTESIAN_POINT ( 'NONE',  ( -2.624999999999996891, -29.95833333333333215, 4.546633369868304797 ) ) ;
#6907 = CARTESIAN_POINT ( 'NONE',  ( -5.114683531250000748, -26.96354166700806587, 2.952963913586931888 ) ) ;
#6908 = CARTESIAN_POINT ( 'NONE',  ( -2.624999999999998668, -28.41666666666666785, -4.546633369868303021 ) ) ;
#6909 = CARTESIAN_POINT ( 'NONE',  ( 5.114683531249999859, -28.40104166700806232, -2.952963913586932776 ) ) ;
#6910 = CARTESIAN_POINT ( 'NONE',  ( -2.625000000000000444, -29.29166666666666785, -4.546633369868303021 ) ) ;
#6911 = CARTESIAN_POINT ( 'NONE',  ( 2.692658234375002735, -29.02604166632526983, 4.663820869356205101 ) ) ;
#6912 = CARTESIAN_POINT ( 'NONE',  ( -5.385316468749998364, -29.58854166632527694, 3.109213912904140287 ) ) ;
#6913 = DIRECTION ( 'NONE',  ( 0.000000000000000000, -0.9973637043974449279, -0.07256473765270717025 ) ) ;
#6914 = CARTESIAN_POINT ( 'NONE',  ( -2.692658234374996518, -28.81770833299193413, 4.663820869356208654 ) ) ;
#6915 = CARTESIAN_POINT ( 'NONE',  ( -2.487701488670255312, -3.649340926099361226, 2.462045979635577808 ) ) ;
#6916 = CARTESIAN_POINT ( 'NONE',  ( -3.492485675378536047, -1.749340926099361093, -1.467888652719048670 ) ) ;
#6917 = EDGE_LOOP ( 'NONE', ( #4587, #7804, #7045, #3820 ) ) ;
#6918 = CARTESIAN_POINT ( 'NONE',  ( 2.324088772396477476E-15, -27.31250000000000000, -5.250000000000000000 ) ) ;
#6919 = CARTESIAN_POINT ( 'NONE',  ( -5.250000000000000888, -27.88541666734946389, 3.031088913245532979 ) ) ;
#6920 = CARTESIAN_POINT ( 'NONE',  ( -5.385316468749998364, -28.83854166632526628, 3.109213912904140287 ) ) ;
#6921 = ORIENTED_EDGE ( 'NONE', *, *, #3278, .F. ) ;
#6922 = CARTESIAN_POINT ( 'NONE',  ( -5.385316468750000141, -28.57812499965860198, 0.000000000000000000 ) ) ;
#6923 = CARTESIAN_POINT ( 'NONE',  ( 2.487701488670203354, -0.3506590739006389956, 2.462045979635629323 ) ) ;
#6924 = FACE_OUTER_BOUND ( 'NONE', #6452, .T. ) ;
#6925 = EDGE_CURVE ( 'NONE', #6499, #7888, #1039, .T. ) ;
#6926 = CARTESIAN_POINT ( 'NONE',  ( -2.625000000000002220, -28.83333333333333215, 4.546633369868302132 ) ) ;
#6927 = CARTESIAN_POINT ( 'NONE',  ( 0.000000000000000000, -30.00000000000000000, 0.000000000000000000 ) ) ;
#6928 = CARTESIAN_POINT ( 'NONE',  ( -3.492485675378535603, -8.149340926099361226, -1.467888652719048670 ) ) ;
#6929 = DIRECTION ( 'NONE',  ( 0.000000000000000000, -1.000000000000000000, 0.000000000000000000 ) ) ;
#6930 = CARTESIAN_POINT ( 'NONE',  ( 1.142306659890740623E-15, -29.01562499965860198, 6.218427825808274356 ) ) ;
#6931 = CARTESIAN_POINT ( 'NONE',  ( 3.507514324621465285, -5.949340926099361937, -1.431606283892619125 ) ) ;
#6932 = DIRECTION ( 'NONE',  ( 0.000000000000000000, -1.000000000000000000, 0.000000000000000000 ) ) ;
#6933 = CARTESIAN_POINT ( 'NONE',  ( -3.807688866302469071E-16, -29.64062499965859843, -6.218427825808274356 ) ) ;
#6934 = CARTESIAN_POINT ( 'NONE',  ( -0.01814118441313417734, -5.750659073900639129, -4.000000000000000000 ) ) ;
#6935 = DIRECTION ( 'NONE',  ( 0.000000000000000000, -1.000000000000000000, 0.000000000000000000 ) ) ;
#6936 = LINE ( 'NONE', #9114, #7145 ) ;
#6937 = VERTEX_POINT ( 'NONE', #1771 ) ;
#6938 = CARTESIAN_POINT ( 'NONE',  ( -2.625000000000000444, -28.54166666666666785, -4.546633369868303021 ) ) ;
#6939 = CARTESIAN_POINT ( 'NONE',  ( 5.114683531250000748, -28.08854166700806232, -2.952963913586932776 ) ) ;
#6940 = CARTESIAN_POINT ( 'NONE',  ( -1.260781871532494103, -2.149340926099361226, 2.992485675378538712 ) ) ;
#6941 = LINE ( 'NONE', #3414, #4355 ) ;
#6942 = CARTESIAN_POINT ( 'NONE',  ( -5.114683531249999859, -27.06770833367473017, -2.952963913586935440 ) ) ;
#6943 = DIRECTION ( 'NONE',  ( 0.000000000000000000, 1.000000000000000000, 0.000000000000000000 ) ) ;
#6944 = CARTESIAN_POINT ( 'NONE',  ( 2.557341765624996821, -29.21354166700806587, 4.429445870380401828 ) ) ;
#6945 = PRODUCT_RELATED_PRODUCT_CATEGORY ( 'part', '', ( #2108 ) ) ;
#6946 =( LENGTH_UNIT ( ) NAMED_UNIT ( * ) SI_UNIT ( .MILLI., .METRE. ) );
#6947 = CARTESIAN_POINT ( 'NONE',  ( 5.114683531250000748, -28.92187500034139802, 0.000000000000000000 ) ) ;
#6948 = CARTESIAN_POINT ( 'NONE',  ( -5.250000000000000000, -28.90625000068279604, -6.429395695523604153E-16 ) ) ;
#6949 = CARTESIAN_POINT ( 'NONE',  ( 2.161402558328724325E-14, -29.31250000000000000, -5.250000000000000000 ) ) ;
#6950 = CARTESIAN_POINT ( 'NONE',  ( 5.250000000000000888, -28.58333333265053611, 3.031088913245532979 ) ) ;
#6951 = CARTESIAN_POINT ( 'NONE',  ( 5.385316468750001029, -29.50520833299193413, 3.109213912904134958 ) ) ;
#6952 = CARTESIAN_POINT ( 'NONE',  ( 0.000000000000000000, 76.00000000000000000, 0.000000000000000000 ) ) ;
#6953 = CARTESIAN_POINT ( 'NONE',  ( 3.492485675378536047, -2.549340926099360694, 1.467888652719046672 ) ) ;
#6954 = CARTESIAN_POINT ( 'NONE',  ( -4.007514324621467949, -5.149340926099361226, 1.638713065079161924 ) ) ;
#6955 = ORIENTED_EDGE ( 'NONE', *, *, #5709, .F. ) ;
#6956 = CARTESIAN_POINT ( 'NONE',  ( 1.045839947578414884E-14, -27.99999999931720041, -5.249999999999999112 ) ) ;
#6957 = CARTESIAN_POINT ( 'NONE',  ( 2.624999999999996891, -26.82291666734946389, 4.546633369868304797 ) ) ;
#6958 = CARTESIAN_POINT ( 'NONE',  ( -5.385316468750001029, -28.88020833299193768, -3.109213912904136734 ) ) ;
#6959 = ADVANCED_FACE ( 'NONE', ( #6602 ), #7999, .T. ) ;
#6960 = EDGE_LOOP ( 'NONE', ( #2425, #5189, #1698, #4017 ) ) ;
#6961 = CARTESIAN_POINT ( 'NONE',  ( 5.385316468750000141, -29.20312499965859843, -6.595110575850215044E-16 ) ) ;
#6962 = CARTESIAN_POINT ( 'NONE',  ( -2.134148098076932953, -5.950659073900640195, -2.108492589042352705 ) ) ;
#6963 = CARTESIAN_POINT ( 'NONE',  ( 5.250000000000000000, -30.00000000000000000, 0.000000000000000000 ) ) ;
#6964 = VECTOR ( 'NONE', #1674, 1000.000000000000000 ) ;
#6965 = ADVANCED_FACE ( 'NONE', ( #7445 ), #8696, .F. ) ;
#6966 = ADVANCED_FACE ( 'NONE', ( #1626 ), #7303, .F. ) ;
#6967 = DIRECTION ( 'NONE',  ( -0.000000000000000000, -0.000000000000000000, 1.000000000000000000 ) ) ;
#6968 = DIRECTION ( 'NONE',  ( 0.000000000000000000, 1.000000000000000000, 0.000000000000000000 ) ) ;
#6969 = CIRCLE ( 'NONE', #2965, 2.050090691792606279 ) ;
#6970 = CARTESIAN_POINT ( 'NONE',  ( -2.557341765624999042, -29.27604166700806232, -4.429445870380400052 ) ) ;
#6971 = CARTESIAN_POINT ( 'NONE',  ( -2.625000000000000444, -28.22916666598386826, -4.546633369868303021 ) ) ;
#6972 = CARTESIAN_POINT ( 'NONE',  ( -1.406733260263384411, -28.73883544963257464, -5.250000000000006217 ) ) ;
#6973 = CARTESIAN_POINT ( 'NONE',  ( -1.467888652719046449, -6.949340926099361049, 3.492485675378536047 ) ) ;
#6974 = CARTESIAN_POINT ( 'NONE',  ( -6.150365299726402968E-16, -50.00000000000000000, 3.794308781941904574 ) ) ;
#6975 = CARTESIAN_POINT ( 'NONE',  ( -2.692658234375000514, -29.86979166632526983, -4.663820869356205989 ) ) ;
#6976 = CARTESIAN_POINT ( 'NONE',  ( -2.841254879263473310, -2.750659073900638685, -2.815599370228907716 ) ) ;
#6977 = CARTESIAN_POINT ( 'NONE',  ( -2.625000000000002220, -27.08333333333333570, 4.546633369868302132 ) ) ;
#6978 = AXIS2_PLACEMENT_3D ( 'NONE', #5263, #3882, #7505 ) ;
#6979 = PRODUCT_DEFINITION_SHAPE ( 'NONE', 'NONE',  #9193 ) ;
#6980 = DIRECTION ( 'NONE',  ( 0.000000000000000000, -0.000000000000000000, 1.000000000000000000 ) ) ;
#6981 = VECTOR ( 'NONE', #721, 1000.000000000000000 ) ;
#6982 = ORIENTED_EDGE ( 'NONE', *, *, #513, .F. ) ;
#6983 =( NAMED_UNIT ( * ) SI_UNIT ( $, .STERADIAN. ) SOLID_ANGLE_UNIT ( ) );
#6984 = CARTESIAN_POINT ( 'NONE',  ( 2.625000000000002220, -28.91666666666666785, 4.546633369868302132 ) ) ;
#6985 = CARTESIAN_POINT ( 'NONE',  ( 5.114683531250000748, -27.35937500034139802, 0.000000000000000000 ) ) ;
#6986 = CARTESIAN_POINT ( 'NONE',  ( 1.260781871532430598, -1.850659073900639884, 2.992485675378564469 ) ) ;
#6987 = CIRCLE ( 'NONE', #6244, 5.250000000000000000 ) ;
#6988 = CARTESIAN_POINT ( 'NONE',  ( -5.114683531250000748, -28.02604166700806587, 2.952963913586931888 ) ) ;
#6989 = ADVANCED_FACE ( 'NONE', ( #6036 ), #8046, .F. ) ;
#6990 = CARTESIAN_POINT ( 'NONE',  ( -5.114683531250000748, -29.06770833367473017, -2.952963913586935440 ) ) ;
#6991 = CIRCLE ( 'NONE', #747, 3.500000000000000444 ) ;
#6992 = SURFACE_STYLE_FILL_AREA ( #1314 ) ;
#6993 = CARTESIAN_POINT ( 'NONE',  ( -5.114683531250000748, -28.77604166700806587, 2.952963913586931888 ) ) ;
#6994 = SHAPE_REPRESENTATION ( 'cone', ( #888 ), #6484 ) ;
#6995 = CARTESIAN_POINT ( 'NONE',  ( 2.625000000000002220, -28.60416666598386826, 4.546633369868302132 ) ) ;
#6996 = CARTESIAN_POINT ( 'NONE',  ( -3.507514324621464397, -0.3493409260993610710, 1.431606283892619347 ) ) ;
#6997 = DIRECTION ( 'NONE',  ( 0.000000000000000000, 0.000000000000000000, 1.000000000000000000 ) ) ;
#6998 = CYLINDRICAL_SURFACE ( 'NONE', #5084, 2.500000000000000444 ) ;
#6999 = CARTESIAN_POINT ( 'NONE',  ( -1.467888652719046449, -5.349340926099361404, 3.492485675378536047 ) ) ;
#7000 = CARTESIAN_POINT ( 'NONE',  ( 2.462045979635577364, -0.8493409260993610710, 2.487701488670255312 ) ) ;
#7001 = ORIENTED_EDGE ( 'NONE', *, *, #3685, .F. ) ;
#7002 = AXIS2_PLACEMENT_3D ( 'NONE', #7329, #955, #1657 ) ;
#7003 = CARTESIAN_POINT ( 'NONE',  ( 0.000000000000000000, -53.00000000000000000, 0.000000000000000000 ) ) ;
#7004 = CARTESIAN_POINT ( 'NONE',  ( 5.114683531249998971, -29.38020833367473017, 2.952963913586936329 ) ) ;
#7005 = CARTESIAN_POINT ( 'NONE',  ( -5.385316468749998364, -30.08854166632526983, 3.109213912904140287 ) ) ;
#7006 = ORIENTED_EDGE ( 'NONE', *, *, #8391, .T. ) ;
#7007 = CARTESIAN_POINT ( 'NONE',  ( -2.692658234374996518, -30.03645833299193413, 4.663820869356208654 ) ) ;
#7008 = CARTESIAN_POINT ( 'NONE',  ( -3.492485675378566246, -4.650659073900639484, 1.467888652718973397 ) ) ;
#7009 = LINE ( 'NONE', #4987, #4149 ) ;
#7010 = DIRECTION ( 'NONE',  ( 0.000000000000000000, 1.000000000000000000, 0.000000000000000000 ) ) ;
#7011 = CARTESIAN_POINT ( 'NONE',  ( 0.000000000000000000, -30.00000000000000000, 5.250000000000000000 ) ) ;
#7012 = PRODUCT_DEFINITION_CONTEXT ( 'detailed design', #3735, 'design' ) ;
#7013 = CARTESIAN_POINT ( 'NONE',  ( 5.114683531249999859, -28.33854166700806587, -2.952963913586932776 ) ) ;
#7014 = CARTESIAN_POINT ( 'NONE',  ( -1.406733260263391960, -28.13616454900183328, 5.250000000000000000 ) ) ;
#7015 = CARTESIAN_POINT ( 'NONE',  ( 1.975475456537005874E-15, -27.87499999931720041, 5.250000000000000000 ) ) ;
#7016 = CARTESIAN_POINT ( 'NONE',  ( 2.108492589042307408, -4.049340926099361582, 2.134148098076978251 ) ) ;
#7017 = EDGE_CURVE ( 'NONE', #3013, #6101, #1766, .T. ) ;
#7018 = CARTESIAN_POINT ( 'NONE',  ( 1.975475456537005874E-15, -28.68749999999999645, 5.250000000000000000 ) ) ;
#7019 = CARTESIAN_POINT ( 'NONE',  ( -5.385316468749998364, -29.80729166632526628, 3.109213912904140287 ) ) ;
#7020 = CARTESIAN_POINT ( 'NONE',  ( -2.841254879263473310, -4.350659073900638774, -2.815599370228907716 ) ) ;
#7021 = CARTESIAN_POINT ( 'NONE',  ( 1.406733260263400176, -28.94866454968462932, -5.249999999999997335 ) ) ;
#7022 = AXIS2_PLACEMENT_3D ( 'NONE', #334, #7601, #2532 ) ;
#7023 = CARTESIAN_POINT ( 'NONE',  ( -2.605717154052086038, -1.491716277579526044E-16, 2.068367651695531162 ) ) ;
#7024 = VERTEX_POINT ( 'NONE', #973 ) ;
#7025 =( NAMED_UNIT ( * ) SI_UNIT ( $, .STERADIAN. ) SOLID_ANGLE_UNIT ( ) );
#7026 = CARTESIAN_POINT ( 'NONE',  ( -2.624999999999996891, -29.45833333333333215, 4.546633369868304797 ) ) ;
#7027 = EDGE_CURVE ( 'NONE', #2212, #7281, #3819, .T. ) ;
#7028 = CIRCLE ( 'NONE', #5092, 5.750000000000000000 ) ;
#7029 = ORIENTED_EDGE ( 'NONE', *, *, #358, .T. ) ;
#7030 = CARTESIAN_POINT ( 'NONE',  ( 3.616337804771879580E-16, -28.29687500034139802, -5.905927827173866440 ) ) ;
#7031 = CARTESIAN_POINT ( 'NONE',  ( 1.224499502706077214, -5.549340926099361582, 3.007514324621463508 ) ) ;
#7032 = CARTESIAN_POINT ( 'NONE',  ( 3.616337804771879580E-16, -27.85937500034139802, -5.905927827173866440 ) ) ;
#7033 = ADVANCED_FACE ( 'NONE', ( #7493 ), #560, .T. ) ;
#7034 = VECTOR ( 'NONE', #5475, 1000.000000000000000 ) ;
#7035 = CIRCLE ( 'NONE', #8670, 5.242490174541154069 ) ;
#7036 = CARTESIAN_POINT ( 'NONE',  ( 5.114683531249998971, -28.69270833367473017, 2.952963913586936329 ) ) ;
#7037 = PRESENTATION_STYLE_ASSIGNMENT (( #4289 ) ) ;
#7038 = CARTESIAN_POINT ( 'NONE',  ( -1.084901341431563923E-15, -28.23437500034139802, 5.905927827173866440 ) ) ;
#7039 = CARTESIAN_POINT ( 'NONE',  ( -2.625000000000000444, -29.47916666598386826, -4.546633369868303021 ) ) ;
#7040 = FACE_OUTER_BOUND ( 'NONE', #8700, .T. ) ;
#7041 = CIRCLE ( 'NONE', #6594, 4.250000000000000000 ) ;
#7042 = DIRECTION ( 'NONE',  ( 0.000000000000000000, 0.000000000000000000, -1.000000000000000000 ) ) ;
#7043 = CARTESIAN_POINT ( 'NONE',  ( -3.507514324621464397, -3.549340926099361582, 1.431606283892619347 ) ) ;
#7044 = CARTESIAN_POINT ( 'NONE',  ( -2.487701488670255312, -3.649340926099361226, 2.462045979635577808 ) ) ;
#7045 = ORIENTED_EDGE ( 'NONE', *, *, #1617, .T. ) ;
#7046 = DIRECTION ( 'NONE',  ( -0.000000000000000000, 1.000000000000000000, -0.000000000000000000 ) ) ;
#7047 = CARTESIAN_POINT ( 'NONE',  ( -5.114683531250000748, -29.23437500034139802, -6.263680815196995234E-16 ) ) ;
#7048 =( BOUNDED_CURVE ( )  B_SPLINE_CURVE ( 2, ( #4461, #5200, #7343, #6546, #8644, #2275, #4417, #1670, #967 ),
 .UNSPECIFIED., .F., .F. ) 
 B_SPLINE_CURVE_WITH_KNOTS ( ( 3, 2, 2, 2, 3 ),
 ( 0.8541666666666667407, 0.8611111111111111605, 0.8750000000000000000, 0.8888888888888888395, 0.8958333333333333703 ),
 .UNSPECIFIED. ) 
 CURVE ( )  GEOMETRIC_REPRESENTATION_ITEM ( )  RATIONAL_B_SPLINE_CURVE ( ( 0.9330127018922192983, 0.9330127018922198534, 1.000000000000000000, 0.8660254037844387076, 1.000000000000000000, 0.8660254037844387076, 1.000000000000000000, 0.9330127018922187432, 0.9330127018922192983 ) ) 
 REPRESENTATION_ITEM ( '' )  );
#7049 = ORIENTED_EDGE ( 'NONE', *, *, #3015, .T. ) ;
#7050 = FACE_OUTER_BOUND ( 'NONE', #1923, .T. ) ;
#7051 = CARTESIAN_POINT ( 'NONE',  ( -2.462045979635629323, -6.350659073900638774, 2.487701488670203798 ) ) ;
#7052 = CARTESIAN_POINT ( 'NONE',  ( 0.000000000000000000, -35.00000000000000000, 0.000000000000000000 ) ) ;
#7053 = EDGE_LOOP ( 'NONE', ( #1806, #4771, #5930, #1744 ) ) ;
#7054 = DIRECTION ( 'NONE',  ( 0.000000000000000000, 1.000000000000000000, 0.000000000000000000 ) ) ;
#7055 = CARTESIAN_POINT ( 'NONE',  ( 0.000000000000000000, 79.00000000000001421, 2.500000000000000000 ) ) ;
#7056 = CARTESIAN_POINT ( 'NONE',  ( 2.624999999999998668, -27.27083333265053611, -4.546633369868303021 ) ) ;
#7057 = CARTESIAN_POINT ( 'NONE',  ( 5.114683531249998971, -28.88020833367473017, 2.952963913586936329 ) ) ;
#7058 = CARTESIAN_POINT ( 'NONE',  ( 1.406733260263398400, -28.26116454900183328, -5.249999999999997335 ) ) ;
#7059 = ITEM_DEFINED_TRANSFORMATION ( 'NONE', 'NONE', #8298,  #888 ) ;
#7060 = CARTESIAN_POINT ( 'NONE',  ( 0.000000000000000000, 1.000000000000000888, -3.000000000000000444 ) ) ;
#7061 = CARTESIAN_POINT ( 'NONE',  ( 2.134148098076978251, -7.649340926099361226, -2.108492589042307408 ) ) ;
#7062 = DIRECTION ( 'NONE',  ( 0.000000000000000000, 0.000000000000000000, -1.000000000000000000 ) ) ;
#7063 = CARTESIAN_POINT ( 'NONE',  ( -2.692658234374996518, -29.28645833299193413, 4.663820869356208654 ) ) ;
#7064 = CARTESIAN_POINT ( 'NONE',  ( 0.01814118441313467001, -1.750659073900638685, 4.000000000000000000 ) ) ;
#7065 = DIRECTION ( 'NONE',  ( 0.000000000000000000, 0.000000000000000000, 1.000000000000000000 ) ) ;
#7066 = CARTESIAN_POINT ( 'NONE',  ( -2.625000000000002220, -26.86458333401613174, 4.546633369868302132 ) ) ;
#7067 = VERTEX_POINT ( 'NONE', #6232 ) ;
#7068 =( LENGTH_UNIT ( ) NAMED_UNIT ( * ) SI_UNIT ( .MILLI., .METRE. ) );
#7069 = CARTESIAN_POINT ( 'NONE',  ( -5.249999999999999112, -29.72916666666667140, 3.031088913245538308 ) ) ;
#7070 = ADVANCED_FACE ( 'NONE', ( #2662 ), #3404, .F. ) ;
#7071 = CARTESIAN_POINT ( 'NONE',  ( 5.114683531249998971, -27.13020833367473372, 2.952963913586936329 ) ) ;
#7072 = CARTESIAN_POINT ( 'NONE',  ( 1.260781871532495657, -6.149340926099362115, -2.992485675378538268 ) ) ;
#7073 = ADVANCED_BREP_SHAPE_REPRESENTATION ( '', ( #2174, #888 ), #6054 ) ;
#7074 = CARTESIAN_POINT ( 'NONE',  ( -5.250000000000000000, -29.64583333333333215, -3.031088913245536531 ) ) ;
#7075 = CARTESIAN_POINT ( 'NONE',  ( 0.000000000000000000, -27.00000000000000000, 0.000000000000000000 ) ) ;
#7076 = EDGE_CURVE ( 'NONE', #2627, #7114, #1952, .T. ) ;
#7077 = CARTESIAN_POINT ( 'NONE',  ( 2.557341765624996821, -29.46354166700806232, 4.429445870380401828 ) ) ;
#7078 = EDGE_CURVE ( 'NONE', #3105, #5259, #6840, .T. ) ;
#7079 = CARTESIAN_POINT ( 'NONE',  ( -2.557341765624999042, -27.08854166700806232, -4.429445870380400052 ) ) ;
#7080 = DIRECTION ( 'NONE',  ( 0.000000000000000000, -1.000000000000000000, 0.000000000000000000 ) ) ;
#7081 = CARTESIAN_POINT ( 'NONE',  ( -3.712013335537174572E-16, -29.74999999931720041, -6.062177826491070398 ) ) ;
#7082 = DIRECTION ( 'NONE',  ( 0.000000000000000000, 0.000000000000000000, -1.000000000000000000 ) ) ;
#7083 = CARTESIAN_POINT ( 'NONE',  ( -2.000431855567539330, -3.316496963571793567E-17, 2.928653597410987075 ) ) ;
#7084 = DIRECTION ( 'NONE',  ( 0.000000000000000000, 0.000000000000000000, 1.000000000000000000 ) ) ;
#7085 = CARTESIAN_POINT ( 'NONE',  ( 3.616337804771879580E-16, -29.85937500034139802, -5.905927827173866440 ) ) ;
#7086 = CARTESIAN_POINT ( 'NONE',  ( -2.462045979635576920, -4.849340926099361404, -2.487701488670255756 ) ) ;
#7087 = ORIENTED_EDGE ( 'NONE', *, *, #768, .T. ) ;
#7088 = FACE_OUTER_BOUND ( 'NONE', #7539, .T. ) ;
#7089 = CARTESIAN_POINT ( 'NONE',  ( 3.712013335537174572E-16, -27.21875000068279604, -6.062177826491070398 ) ) ;
#7090 = ORIENTED_EDGE ( 'NONE', *, *, #8447, .F. ) ;
#7091 = VERTEX_POINT ( 'NONE', #6974 ) ;
#7092 = CARTESIAN_POINT ( 'NONE',  ( 1.142306659890740623E-15, -29.26562499965859843, 6.218427825808274356 ) ) ;
#7093 = CARTESIAN_POINT ( 'NONE',  ( 3.492485675378566690, -3.850659073900639218, -1.467888652718972287 ) ) ;
#7094 = DIRECTION ( 'NONE',  ( 0.000000000000000000, 0.000000000000000000, -1.000000000000000000 ) ) ;
#7095 = ORIENTED_EDGE ( 'NONE', *, *, #2297, .F. ) ;
#7096 = ADVANCED_FACE ( 'NONE', ( #515 ), #6139, .T. ) ;
#7097 = LINE ( 'NONE', #9143, #6981 ) ;
#7098 = DIRECTION ( 'NONE',  ( 0.000000000000000000, -1.000000000000000000, 0.000000000000000000 ) ) ;
#7099 = EDGE_CURVE ( 'NONE', #6502, #5775, #7566, .T. ) ;
#7100 = DIRECTION ( 'NONE',  ( -0.000000000000000000, 1.000000000000000000, -0.000000000000000000 ) ) ;
#7101 = CARTESIAN_POINT ( 'NONE',  ( 3.616337804771879580E-16, -28.29687500034139802, -5.905927827173866440 ) ) ;
#7102 = CYLINDRICAL_SURFACE ( 'NONE', #1093, 5.250000000000000000 ) ;
#7103 = ITEM_DEFINED_TRANSFORMATION ( 'NONE', 'NONE', #4727,  #888 ) ;
#7104 = DIRECTION ( 'NONE',  ( -0.8660254037844402619, -0.4999999999999970579, 0.000000000000000000 ) ) ;
#7105 = CARTESIAN_POINT ( 'NONE',  ( -2.992485675378538268, -4.949340926099361937, -1.260781871532495879 ) ) ;
#7106 = FACE_OUTER_BOUND ( 'NONE', #4533, .T. ) ;
#7107 = CARTESIAN_POINT ( 'NONE',  ( -2.692658234374996518, -27.56770833299193413, 4.663820869356208654 ) ) ;
#7108 = CARTESIAN_POINT ( 'NONE',  ( -1.638713065079245634, -1.650659073900638818, 4.007514324621432422 ) ) ;
#7109 = PRESENTATION_STYLE_ASSIGNMENT (( #4277 ) ) ;
#7110 = AXIS2_PLACEMENT_3D ( 'NONE', #4318, #686, #6314 ) ;
#7111 = DIRECTION ( 'NONE',  ( 0.000000000000000000, 1.000000000000000000, 0.000000000000000000 ) ) ;
#7112 = ORIENTED_EDGE ( 'NONE', *, *, #3553, .F. ) ;
#7113 = CARTESIAN_POINT ( 'NONE',  ( -3.807688866302469071E-16, -27.39062499965860198, -6.218427825808274356 ) ) ;
#7114 = VERTEX_POINT ( 'NONE', #6786 ) ;
#7115 = CIRCLE ( 'NONE', #4746, 1.749999999999999778 ) ;
#7116 = CARTESIAN_POINT ( 'NONE',  ( -5.385316468750001029, -27.09895833299193413, -3.109213912904136734 ) ) ;
#7117 = CARTESIAN_POINT ( 'NONE',  ( 0.01814118441314514080, -0.1506590739006394009, 3.000000000000000444 ) ) ;
#7118 = ORIENTED_EDGE ( 'NONE', *, *, #7770, .F. ) ;
#7119 = CARTESIAN_POINT ( 'NONE',  ( 3.712013335537174572E-16, -29.18750000000000000, -6.062177826491070398 ) ) ;
#7120 = CARTESIAN_POINT ( 'NONE',  ( 0.000000000000000000, -27.00000000000000000, 0.000000000000000000 ) ) ;
#7121 =( BOUNDED_CURVE ( )  B_SPLINE_CURVE ( 2, ( #7923, #8060, #842, #2246, #942, #8708, #3644, #985, #2294 ),
 .UNSPECIFIED., .F., .T. ) 
 B_SPLINE_CURVE_WITH_KNOTS ( ( 3, 2, 2, 2, 3 ),
 ( 0.3958333333333333703, 0.4027777777777777901, 0.4166666666666666852, 0.4305555555555555802, 0.4375000000000000000 ),
 .UNSPECIFIED. ) 
 CURVE ( )  GEOMETRIC_REPRESENTATION_ITEM ( )  RATIONAL_B_SPLINE_CURVE ( ( 0.9330127018922194093, 0.9330127018922196314, 1.000000000000000000, 0.8660254037844387076, 1.000000000000000000, 0.8660254037844387076, 1.000000000000000000, 0.9330127018922194093, 0.9330127018922194093 ) ) 
 REPRESENTATION_ITEM ( '' )  );
#7122 = CARTESIAN_POINT ( 'NONE',  ( 5.114683531249998971, -28.19270833367473017, 2.952963913586936329 ) ) ;
#7123 = AXIS2_PLACEMENT_3D ( 'NONE', #3643, #2952, #6513 ) ;
#7124 = CLOSED_SHELL ( 'NONE', ( #206, #5426, #8362, #6822, #971, #6238, #194, #4133, #481, #6751, #5483, #6965, #7486, #8941, #1867, #1436, #3692, #486, #7675, #6858, #7704, #713, #7070, #1169, #3621, #4957, #5164, #7358, #4343, #5618, #6550, #3850, #8677, #8212, #5374, #6966, #4659, #4190, #5878, #3886 ) ) ;
#7125 = CARTESIAN_POINT ( 'NONE',  ( 5.114683531250000748, -27.17187500034139802, 0.000000000000000000 ) ) ;
#7126 = CIRCLE ( 'NONE', #5037, 1.499999999999999778 ) ;
#7127 = CARTESIAN_POINT ( 'NONE',  ( 1.113604000661152470E-15, -29.12499999931720751, 6.062177826491070398 ) ) ;
#7128 = CARTESIAN_POINT ( 'NONE',  ( 2.624999999999998668, -27.52083333265053611, -4.546633369868303021 ) ) ;
#7129 = EDGE_CURVE ( 'NONE', #1374, #7067, #603, .T. ) ;
#7130 = CARTESIAN_POINT ( 'NONE',  ( 2.624999999999996891, -29.57291666734946034, 4.546633369868304797 ) ) ;
#7131 = CARTESIAN_POINT ( 'NONE',  ( 1.406733260263405061, -28.44866454968462932, -5.249999999999994671 ) ) ;
#7132 = CARTESIAN_POINT ( 'NONE',  ( -1.406733260263395735, -29.60491455036742892, 5.250000000000000000 ) ) ;
#7133 = CLOSED_SHELL ( 'NONE', ( #7096, #1386, #3796, #8797, #5704, #2877, #6174, #5872, #7979 ) ) ;
#7134 = CARTESIAN_POINT ( 'NONE',  ( 1.467888652719048226, -4.549340926099360694, -3.492485675378536047 ) ) ;
#7135 = ORIENTED_EDGE ( 'NONE', *, *, #3135, .T. ) ;
#7136 = CARTESIAN_POINT ( 'NONE',  ( 5.249999999999999112, -28.04166666598386826, -3.031088913245536975 ) ) ;
#7137 = CARTESIAN_POINT ( 'NONE',  ( 0.000000000000000000, -29.00000000000000355, 0.000000000000000000 ) ) ;
#7138 = CIRCLE ( 'NONE', #3133, 4.000000000000000000 ) ;
#7139 = CARTESIAN_POINT ( 'NONE',  ( 2.557341765624996821, -29.65104166700806232, 4.429445870380401828 ) ) ;
#7140 = ORIENTED_EDGE ( 'NONE', *, *, #5709, .T. ) ;
#7141 = ORIENTED_EDGE ( 'NONE', *, *, #2253, .T. ) ;
#7142 = CARTESIAN_POINT ( 'NONE',  ( 1.142306659890740623E-15, -30.01562499965859843, 6.218427825808274356 ) ) ;
#7143 = CARTESIAN_POINT ( 'NONE',  ( -3.500000000000000000, -7.750659073900639129, 0.01814118441314012051 ) ) ;
#7144 = CARTESIAN_POINT ( 'NONE',  ( 1.975475456537005874E-15, -27.62499999931720041, 5.249999999999999112 ) ) ;
#7145 = VECTOR ( 'NONE', #4655, 1000.000000000000000 ) ;
#7146 = VERTEX_POINT ( 'NONE', #5534 ) ;
#7147 = CARTESIAN_POINT ( 'NONE',  ( 0.000000000000000000, -30.00000000000000000, 0.000000000000000000 ) ) ;
#7148 = CARTESIAN_POINT ( 'NONE',  ( 5.385316468750001029, -27.25520833299193413, 3.109213912904135846 ) ) ;
#7149 = CARTESIAN_POINT ( 'NONE',  ( 2.557341765624996821, -28.65104166700806587, 4.429445870380401828 ) ) ;
#7150 = EDGE_CURVE ( 'NONE', #2693, #4496, #982, .T. ) ;
#7151 = CARTESIAN_POINT ( 'NONE',  ( 3.500000000000000000, -1.049340926099360916, 0.01814118441321387054 ) ) ;
#7152 = CARTESIAN_POINT ( 'NONE',  ( 1.406733260263395735, -27.86383544963257464, 5.250000000000000000 ) ) ;
#7153 = CARTESIAN_POINT ( 'NONE',  ( 2.134148098076978251, -2.849340926099362292, -2.108492589042307408 ) ) ;
#7154 = CARTESIAN_POINT ( 'NONE',  ( 5.114683531250000748, -29.85937500034139802, 0.000000000000000000 ) ) ;
#7155 = CARTESIAN_POINT ( 'NONE',  ( 2.692658234375002735, -28.02604166632526628, 4.663820869356205101 ) ) ;
#7156 = CARTESIAN_POINT ( 'NONE',  ( 4.000000000000000000, -1.049340926099360916, 0.01814118441321914063 ) ) ;
#7157 = DIRECTION ( 'NONE',  ( 0.000000000000000000, 1.000000000000000000, 0.000000000000000000 ) ) ;
#7158 = CARTESIAN_POINT ( 'NONE',  ( 2.300847884672513123E-14, -28.21875000068279604, -5.250000000000000000 ) ) ;
#7159 = VERTEX_POINT ( 'NONE', #8190 ) ;
#7160 = CARTESIAN_POINT ( 'NONE',  ( 5.385316468749999252, -27.43229166632526983, -3.109213912904139399 ) ) ;
#7161 = EDGE_LOOP ( 'NONE', ( #3140, #2991 ) ) ;
#7162 = CARTESIAN_POINT ( 'NONE',  ( 1.975475456537005874E-15, -27.18750000000000000, 5.250000000000000000 ) ) ;
#7163 = CARTESIAN_POINT ( 'NONE',  ( -2.992485675378564469, -1.450659073900639751, 1.260781871532430820 ) ) ;
#7164 = ORIENTED_EDGE ( 'NONE', *, *, #9163, .F. ) ;
#7165 = CARTESIAN_POINT ( 'NONE',  ( -2.625000000000002220, -29.83333333333333215, 4.546633369868302132 ) ) ;
#7166 = DIRECTION ( 'NONE',  ( 0.000000000000000000, 0.000000000000000000, -1.000000000000000000 ) ) ;
#7167 = EDGE_CURVE ( 'NONE', #7319, #6852, #4199, .T. ) ;
#7168 = CARTESIAN_POINT ( 'NONE',  ( 5.114683531249998971, -27.94270833367473017, 2.952963913586936329 ) ) ;
#7169 = AXIS2_PLACEMENT_3D ( 'NONE', #1177, #6904, #528 ) ;
#7170 =( NAMED_UNIT ( * ) PLANE_ANGLE_UNIT ( ) SI_UNIT ( $, .RADIAN. ) );
#7171 = CARTESIAN_POINT ( 'NONE',  ( 2.557341765624996821, -27.71354166700806587, 4.429445870380401828 ) ) ;
#7172 = CARTESIAN_POINT ( 'NONE',  ( 1.113604000661152470E-15, -30.12499999931720041, 6.062177826491070398 ) ) ;
#7173 = DIRECTION ( 'NONE',  ( 0.000000000000000000, 0.000000000000000000, 1.000000000000000000 ) ) ;
#7174 = CARTESIAN_POINT ( 'NONE',  ( 0.000000000000000000, 79.00000000000001421, 0.000000000000000000 ) ) ;
#7175 = AXIS2_PLACEMENT_3D ( 'NONE', #8039, #6637, #5287 ) ;
#7176 = FACE_BOUND ( 'NONE', #6664, .T. ) ;
#7177 = CARTESIAN_POINT ( 'NONE',  ( 2.557341765625000818, -29.63020833367473017, -4.429445870380400052 ) ) ;
#7178 = CARTESIAN_POINT ( 'NONE',  ( 3.507514324621465285, -7.549340926099362470, -1.431606283892619125 ) ) ;
#7179 = AXIS2_PLACEMENT_3D ( 'NONE', #1366, #4892, #7173 ) ;
#7180 = VERTEX_POINT ( 'NONE', #8239 ) ;
#7181 = CARTESIAN_POINT ( 'NONE',  ( -2.625000000000002220, -28.61458333401612819, 4.546633369868302132 ) ) ;
#7182 = DIRECTION ( 'NONE',  ( 0.000000000000000000, 0.000000000000000000, 1.000000000000000000 ) ) ;
#7183 = CARTESIAN_POINT ( 'NONE',  ( 5.114683531250000748, -27.85937500034139802, 0.000000000000000000 ) ) ;
#7184 = VERTEX_POINT ( 'NONE', #2754 ) ;
#7185 = AXIS2_PLACEMENT_3D ( 'NONE', #6882, #8917, #7529 ) ;
#7186 = VERTEX_POINT ( 'NONE', #1962 ) ;
#7187 = DIRECTION ( 'NONE',  ( 0.000000000000000000, 1.000000000000000000, 0.000000000000000000 ) ) ;
#7188 = CARTESIAN_POINT ( 'NONE',  ( -3.807688866302469071E-16, -27.67187499965860198, -6.218427825808274356 ) ) ;
#7189 = CARTESIAN_POINT ( 'NONE',  ( 0.01814118441313990887, -4.950659073900639306, 3.500000000000000000 ) ) ;
#7190 = CARTESIAN_POINT ( 'NONE',  ( -1.406733260263395735, -29.07366454968462577, 5.250000000000000000 ) ) ;
#7191 = ORIENTED_EDGE ( 'NONE', *, *, #2445, .T. ) ;
#7192 = CARTESIAN_POINT ( 'NONE',  ( 2.625000000000000444, -29.23958333401613174, -4.546633369868303021 ) ) ;
#7193 = FACE_OUTER_BOUND ( 'NONE', #5303, .T. ) ;
#7194 = CARTESIAN_POINT ( 'NONE',  ( -2.557341765625002594, -27.44270833367473017, 4.429445870380399164 ) ) ;
#7195 = CARTESIAN_POINT ( 'NONE',  ( 1.431606283892619125, -0.7493409260993610932, 3.507514324621464397 ) ) ;
#7196 = DIRECTION ( 'NONE',  ( 1.000000000000000000, 0.000000000000000000, 0.000000000000000000 ) ) ;
#7197 = EDGE_CURVE ( 'NONE', #3585, #8002, #1394, .T. ) ;
#7198 = CARTESIAN_POINT ( 'NONE',  ( 1.224499502706077214, -2.349340926099361848, 3.007514324621463508 ) ) ;
#7199 = CYLINDRICAL_SURFACE ( 'NONE', #3112, 5.250000000000000000 ) ;
#7200 = CARTESIAN_POINT ( 'NONE',  ( 5.385316468750001029, -28.00520833299193413, 3.109213912904135846 ) ) ;
#7201 = CARTESIAN_POINT ( 'NONE',  ( -1.638713065079245634, -6.450659073900638418, 4.007514324621432422 ) ) ;
#7202 = LINE ( 'NONE', #781, #2697 ) ;
#7203 = CARTESIAN_POINT ( 'NONE',  ( 2.033577675846918216E-14, -27.59375000068279959, 5.250000000000000888 ) ) ;
#7204 = CARTESIAN_POINT ( 'NONE',  ( 1.406733260263403507, -29.01116454900182973, -5.249999999999994671 ) ) ;
#7205 = EDGE_LOOP ( 'NONE', ( #8715, #3181, #764, #4257 ) ) ;
#7206 = CARTESIAN_POINT ( 'NONE',  ( 2.692658234374998738, -27.16145833299193413, -4.663820869356206877 ) ) ;
#7207 = VERTEX_POINT ( 'NONE', #7719 ) ;
#7208 = CARTESIAN_POINT ( 'NONE',  ( -5.385316468749998364, -27.55729166632526628, 3.109213912904140287 ) ) ;
#7209 = CARTESIAN_POINT ( 'NONE',  ( 1.224499502706142273, -5.650659073900639484, -3.007514324621435531 ) ) ;
#7210 = ORIENTED_EDGE ( 'NONE', *, *, #783, .F. ) ;
#7211 = CARTESIAN_POINT ( 'NONE',  ( -2.625000000000002220, -29.58333333333333215, 4.546633369868302132 ) ) ;
#7212 = CARTESIAN_POINT ( 'NONE',  ( 1.406733260263395735, -29.42633545031537423, 5.250000000000000000 ) ) ;
#7213 = CARTESIAN_POINT ( 'NONE',  ( -5.114683531250000748, -28.04687500034139802, -6.263680815196995234E-16 ) ) ;
#7214 = CARTESIAN_POINT ( 'NONE',  ( 3.616337804771879580E-16, -27.60937500034139802, -5.905927827173866440 ) ) ;
#7215 = CARTESIAN_POINT ( 'NONE',  ( 3.673940397442059375E-16, -46.00000000000000000, 2.999999999999999556 ) ) ;
#7216 = CARTESIAN_POINT ( 'NONE',  ( 0.01814118441321408565, -1.449340926099361271, -3.500000000000000000 ) ) ;
#7217 = CARTESIAN_POINT ( 'NONE',  ( 5.249999999999999112, -28.76041666734946389, -3.031088913245534755 ) ) ;
#7218 = CARTESIAN_POINT ( 'NONE',  ( -0.01814118441321365544, -7.049340926099361582, 3.500000000000000000 ) ) ;
#7219 = CARTESIAN_POINT ( 'NONE',  ( -3.500000000000000000, -5.049340926099361582, -0.01814118441321344033 ) ) ;
#7220 = ORIENTED_EDGE ( 'NONE', *, *, #4097, .T. ) ;
#7221 = CARTESIAN_POINT ( 'NONE',  ( -0.01814118441313947866, -5.750659073900639129, -3.500000000000000000 ) ) ;
#7222 = CARTESIAN_POINT ( 'NONE',  ( 2.625000000000000444, -26.98958333401612819, -4.546633369868303021 ) ) ;
#7223 = CARTESIAN_POINT ( 'NONE',  ( -5.114683531249999859, -29.00520833367473017, -2.952963913586935440 ) ) ;
#7224 = ORIENTED_EDGE ( 'NONE', *, *, #4302, .T. ) ;
#7225 = VERTEX_POINT ( 'NONE', #6223 ) ;
#7226 = CARTESIAN_POINT ( 'NONE',  ( -2.624999999999996891, -29.70833333333333215, 4.546633369868304797 ) ) ;
#7227 = CARTESIAN_POINT ( 'NONE',  ( -2.692658234375000514, -27.15104166632526628, -4.663820869356205989 ) ) ;
#7228 = CARTESIAN_POINT ( 'NONE',  ( 0.01814118441313467001, -6.550659073900640728, 4.000000000000000000 ) ) ;
#7229 = CARTESIAN_POINT ( 'NONE',  ( 7.654042494670957606E-16, 76.00000000000000000, -6.250000000000000000 ) ) ;
#7230 = ORIENTED_EDGE ( 'NONE', *, *, #1645, .T. ) ;
#7231 = PRODUCT_DEFINITION_SHAPE ( 'NONE', 'NONE',  #8320 ) ;
#7232 = CARTESIAN_POINT ( 'NONE',  ( -2.625000000000002220, -29.83333333333333215, 4.546633369868302132 ) ) ;
#7233 = CARTESIAN_POINT ( 'NONE',  ( 5.250000000000000000, -29.76041666734946034, -3.031088913245534755 ) ) ;
#7234 = ADVANCED_FACE ( 'NONE', ( #2135 ), #1521, .T. ) ;
#7235 = CARTESIAN_POINT ( 'NONE',  ( -3.807688866302469071E-16, -27.42187499965860198, -6.218427825808274356 ) ) ;
#7236 = CARTESIAN_POINT ( 'NONE',  ( -5.114683531250000748, -27.21354166700806587, 2.952963913586931888 ) ) ;
#7237 = FACE_BOUND ( 'NONE', #88, .T. ) ;
#7238 = DIRECTION ( 'NONE',  ( 0.000000000000000000, 0.000000000000000000, 1.000000000000000000 ) ) ;
#7239 = CARTESIAN_POINT ( 'NONE',  ( 1.224499502706142273, -4.050659073900639839, -3.007514324621435531 ) ) ;
#7240 = DIRECTION ( 'NONE',  ( 0.000000000000000000, 0.000000000000000000, 1.000000000000000000 ) ) ;
#7241 =( GEOMETRIC_REPRESENTATION_CONTEXT ( 3 ) GLOBAL_UNCERTAINTY_ASSIGNED_CONTEXT ( ( #7475 ) ) GLOBAL_UNIT_ASSIGNED_CONTEXT ( ( #7774, #9155, #8426 ) ) REPRESENTATION_CONTEXT ( 'NONE', 'WORKASPACE' ) );
#7242 = CARTESIAN_POINT ( 'NONE',  ( -1.674995433905599462, -3.749340926099360871, 3.992485675378533383 ) ) ;
#7243 = EDGE_CURVE ( 'NONE', #2713, #8000, #123, .T. ) ;
#7244 = CARTESIAN_POINT ( 'NONE',  ( -3.712013335537174572E-16, -27.49999999931720041, -6.062177826491070398 ) ) ;
#7245 = CARTESIAN_POINT ( 'NONE',  ( -2.625000000000000444, -27.04166666666666430, -4.546633369868303021 ) ) ;
#7246 = CARTESIAN_POINT ( 'NONE',  ( 6.429395695523604153E-16, 69.99999999999998579, -5.250000000000000000 ) ) ;
#7247 = FACE_OUTER_BOUND ( 'NONE', #6321, .T. ) ;
#7248 = ORIENTED_EDGE ( 'NONE', *, *, #7462, .F. ) ;
#7249 = DIRECTION ( 'NONE',  ( 0.000000000000000000, 0.000000000000000000, 1.000000000000000000 ) ) ;
#7250 = CARTESIAN_POINT ( 'NONE',  ( 5.385316468749999252, -27.68229166632526272, -3.109213912904139399 ) ) ;
#7251 = CARTESIAN_POINT ( 'NONE',  ( 1.674995433905601239, -6.149340926099362115, -3.992485675378532939 ) ) ;
#7252 = CARTESIAN_POINT ( 'NONE',  ( 2.161402558328724325E-14, -29.56250000000000355, -5.250000000000000000 ) ) ;
#7253 = ORIENTED_EDGE ( 'NONE', *, *, #8142, .T. ) ;
#7254 = CARTESIAN_POINT ( 'NONE',  ( 0.000000000000000000, -27.00000000000000000, 0.000000000000000000 ) ) ;
#7255 = CARTESIAN_POINT ( 'NONE',  ( 2.992485675378565357, -3.850659073900639662, -1.260781871532430376 ) ) ;
#7256 = VERTEX_POINT ( 'NONE', #4185 ) ;
#7257 = CARTESIAN_POINT ( 'NONE',  ( -2.624999999999998668, -29.16666666666666785, -4.546633369868303021 ) ) ;
#7258 = AXIS2_PLACEMENT_3D ( 'NONE', #3151, #6863, #5969 ) ;
#7259 = CARTESIAN_POINT ( 'NONE',  ( -2.557341765625002594, -27.25520833367473017, 4.429445870380399164 ) ) ;
#7260 = SURFACE_STYLE_USAGE ( .BOTH. , #6560 ) ;
#7261 = VECTOR ( 'NONE', #1420, 1000.000000000000000 ) ;
#7262 = CARTESIAN_POINT ( 'NONE',  ( -5.249999999999999112, -27.72916666666666785, 3.031088913245538308 ) ) ;
#7263 = CARTESIAN_POINT ( 'NONE',  ( -5.250000000000000000, -29.95833333265053611, -3.031088913245534755 ) ) ;
#7264 = CARTESIAN_POINT ( 'NONE',  ( -3.507514324621464397, -6.749340926099361759, 1.431606283892619347 ) ) ;
#7265 = CARTESIAN_POINT ( 'NONE',  ( 2.625000000000000444, -28.73958333401612819, -4.546633369868303021 ) ) ;
#7266 = DIRECTION ( 'NONE',  ( -0.000000000000000000, -1.000000000000000000, -0.000000000000000000 ) ) ;
#7267 = CARTESIAN_POINT ( 'NONE',  ( 5.114683531249999859, -29.90104166700806232, -2.952963913586932776 ) ) ;
#7268 = SURFACE_STYLE_USAGE ( .BOTH. , #4433 ) ;
#7269 = EDGE_CURVE ( 'NONE', #8711, #2434, #5134, .T. ) ;
#7270 = ORIENTED_EDGE ( 'NONE', *, *, #3505, .F. ) ;
#7271 = CARTESIAN_POINT ( 'NONE',  ( 2.625000000000002220, -28.10416666598386826, 4.546633369868302132 ) ) ;
#7272 = FACE_OUTER_BOUND ( 'NONE', #2896, .T. ) ;
#7273 = CARTESIAN_POINT ( 'NONE',  ( 5.114683531249999859, -28.33854166700806587, -2.952963913586932776 ) ) ;
#7274 = AXIS2_PLACEMENT_3D ( 'NONE', #7710, #5609, #4862 ) ;
#7275 = VERTEX_POINT ( 'NONE', #7154 ) ;
#7276 = CIRCLE ( 'NONE', #8907, 1.499999999999999778 ) ;
#7277 = LINE ( 'NONE', #1652, #1105 ) ;
#7278 = CARTESIAN_POINT ( 'NONE',  ( -2.692658234374996518, -27.81770833299193413, 4.663820869356208654 ) ) ;
#7279 = CARTESIAN_POINT ( 'NONE',  ( -2.815599370228907272, -3.150659073900639040, 2.841254879263473754 ) ) ;
#7280 = DIRECTION ( 'NONE',  ( -0.000000000000000000, -0.000000000000000000, 1.000000000000000000 ) ) ;
#7281 = VERTEX_POINT ( 'NONE', #1429 ) ;
#7282 = AXIS2_PLACEMENT_3D ( 'NONE', #4690, #5429, #4825 ) ;
#7283 = CARTESIAN_POINT ( 'NONE',  ( -5.250000000000000000, -27.93749999931720396, 0.000000000000000000 ) ) ;
#7284 = CARTESIAN_POINT ( 'NONE',  ( -1.113604000661152470E-15, -29.34375000068279604, 6.062177826491070398 ) ) ;
#7285 = CARTESIAN_POINT ( 'NONE',  ( -3.807688866302469071E-16, -27.92187499965860198, -6.218427825808274356 ) ) ;
#7286 = CARTESIAN_POINT ( 'NONE',  ( 2.557341765624996821, -27.65104166700806587, 4.429445870380401828 ) ) ;
#7287 = CARTESIAN_POINT ( 'NONE',  ( 0.000000000000000000, -46.00000000000000000, 0.000000000000000000 ) ) ;
#7288 = AXIS2_PLACEMENT_3D ( 'NONE', #7593, #2759, #1303 ) ;
#7289 = CARTESIAN_POINT ( 'NONE',  ( 1.142306659890740623E-15, -27.51562499965860198, 6.218427825808274356 ) ) ;
#7290 = CARTESIAN_POINT ( 'NONE',  ( 0.01814118441314514080, -0.1506590739006394009, 3.000000000000000444 ) ) ;
#7291 = UNCERTAINTY_MEASURE_WITH_UNIT (LENGTH_MEASURE( 1.000000000000000082E-05 ), #3510, 'distance_accuracy_value', 'NONE');
#7292 = DIRECTION ( 'NONE',  ( -0.000000000000000000, -0.000000000000000000, 1.000000000000000000 ) ) ;
#7293 = CARTESIAN_POINT ( 'NONE',  ( -3.992485675378568022, -6.250659073900639129, 1.674995433905515529 ) ) ;
#7294 = CARTESIAN_POINT ( 'NONE',  ( -5.250000000000000000, -27.68749999931720396, 0.000000000000000000 ) ) ;
#7295 = CARTESIAN_POINT ( 'NONE',  ( 2.033577675846918216E-14, -27.59375000068279604, 5.250000000000000888 ) ) ;
#7296 = CARTESIAN_POINT ( 'NONE',  ( -3.507514324621464397, -3.549340926099361138, 1.431606283892619569 ) ) ;
#7297 = LINE ( 'NONE', #921, #2083 ) ;
#7298 = EDGE_CURVE ( 'NONE', #2142, #6825, #9150, .T. ) ;
#7299 = ORIENTED_EDGE ( 'NONE', *, *, #7099, .T. ) ;
#7300 =( NAMED_UNIT ( * ) PLANE_ANGLE_UNIT ( ) SI_UNIT ( $, .RADIAN. ) );
#7301 = CARTESIAN_POINT ( 'NONE',  ( -2.692658234375000514, -28.61979166632526628, -4.663820869356205989 ) ) ;
#7302 = CARTESIAN_POINT ( 'NONE',  ( -0.01814118441321889430, -7.049340926099361582, 4.000000000000000000 ) ) ;
#7303 = PLANE ( 'NONE',  #7406 ) ;
#7304 = EDGE_LOOP ( 'NONE', ( #7307, #7220, #7931, #902, #4983, #4042, #5668, #2080, #1662, #4729, #7112, #3296, #5294, #3680, #1919, #4724, #5516, #7660, #8830, #3031, #274, #132, #1780, #23, #4172, #6215, #1535, #2918 ) ) ;
#7305 = CARTESIAN_POINT ( 'NONE',  ( 0.000000000000000000, 81.00000000000001421, -4.000000000000000000 ) ) ;
#7306 = CARTESIAN_POINT ( 'NONE',  ( 3.507514324621434199, -0.4506590739006390844, 1.431606283892693066 ) ) ;
#7307 = ORIENTED_EDGE ( 'NONE', *, *, #5917, .T. ) ;
#7308 = CARTESIAN_POINT ( 'NONE',  ( 2.624999999999996891, -27.29166666666666430, 4.546633369868304797 ) ) ;
#7309 = CARTESIAN_POINT ( 'NONE',  ( 2.557341765624996821, -28.46354166700806587, 4.429445870380401828 ) ) ;
#7310 = EDGE_CURVE ( 'NONE', #8090, #6529, #126, .T. ) ;
#7311 =( NAMED_UNIT ( * ) SI_UNIT ( $, .STERADIAN. ) SOLID_ANGLE_UNIT ( ) );
#7312 = CARTESIAN_POINT ( 'NONE',  ( -2.624999999999996891, -27.20833333333333570, 4.546633369868304797 ) ) ;
#7313 = EDGE_CURVE ( 'NONE', #6937, #5826, #3547, .T. ) ;
#7314 = CYLINDRICAL_SURFACE ( 'NONE', #1089, 5.250000000000000000 ) ;
#7315 = CARTESIAN_POINT ( 'NONE',  ( -3.500000000000000000, -1.849340926099361182, -0.01814118441321344033 ) ) ;
#7316 = CARTESIAN_POINT ( 'NONE',  ( -1.406733260263389518, -27.80133545031536357, -5.250000000000001776 ) ) ;
#7317 = CARTESIAN_POINT ( 'NONE',  ( -2.557341765624999042, -29.33854166700806232, -4.429445870380400052 ) ) ;
#7318 = DIRECTION ( 'NONE',  ( 0.000000000000000000, 0.000000000000000000, -1.000000000000000000 ) ) ;
#7319 = VERTEX_POINT ( 'NONE', #3532 ) ;
#7320 = CARTESIAN_POINT ( 'NONE',  ( -1.975475456537005874E-15, -29.34375000068279249, 5.249999999999999112 ) ) ;
#7321 = CARTESIAN_POINT ( 'NONE',  ( 2.557341765624996821, -28.40104166700806587, 4.429445870380401828 ) ) ;
#7322 = VERTEX_POINT ( 'NONE', #729 ) ;
#7323 = CARTESIAN_POINT ( 'NONE',  ( 0.000000000000000000, -29.00000000000000355, 0.000000000000000000 ) ) ;
#7324 = CARTESIAN_POINT ( 'NONE',  ( 5.385316468750001029, -28.00520833299193768, 3.109213912904134958 ) ) ;
#7325 = CARTESIAN_POINT ( 'NONE',  ( 2.815599370228907716, -5.550659073900638063, -2.841254879263473310 ) ) ;
#7326 = CIRCLE ( 'NONE', #1683, 4.199909308207394609 ) ;
#7327 = CARTESIAN_POINT ( 'NONE',  ( 5.250000000000000000, -29.31249999931720041, -6.429395695523604153E-16 ) ) ;
#7328 = EDGE_LOOP ( 'NONE', ( #2309, #1157, #954, #4462 ) ) ;
#7329 = CARTESIAN_POINT ( 'NONE',  ( 0.000000000000000000, -20.00000000000000000, 0.000000000000000000 ) ) ;
#7330 = VECTOR ( 'NONE', #6350, 1000.000000000000000 ) ;
#7331 = CARTESIAN_POINT ( 'NONE',  ( 5.249999999999999112, -28.80208333401612819, 3.031088913245538308 ) ) ;
#7332 = CARTESIAN_POINT ( 'NONE',  ( -2.692658234374996518, -27.81770833299193413, 4.663820869356208654 ) ) ;
#7333 = CARTESIAN_POINT ( 'NONE',  ( 2.557341765624996821, -29.71354166700806232, 4.429445870380401828 ) ) ;
#7334 = ORIENTED_EDGE ( 'NONE', *, *, #2325, .F. ) ;
#7335 = CARTESIAN_POINT ( 'NONE',  ( -5.385316468750000141, -27.32812499965860198, 0.000000000000000000 ) ) ;
#7336 = CARTESIAN_POINT ( 'NONE',  ( 2.134148098076933397, -3.550659073900639395, 2.108492589042352261 ) ) ;
#7337 = CARTESIAN_POINT ( 'NONE',  ( 5.182341765625000818, -29.96093750017069723, 0.000000000000000000 ) ) ;
#7338 = CARTESIAN_POINT ( 'NONE',  ( -4.000000000000000000, -3.449340926099361049, -0.01814118441321865144 ) ) ;
#7339 = CARTESIAN_POINT ( 'NONE',  ( 5.250000000000000000, -28.06249999931720396, -6.429395695523604153E-16 ) ) ;
#7340 = CARTESIAN_POINT ( 'NONE',  ( 3.673940397442060361E-16, 70.00000000000000000, 3.000000000000000444 ) ) ;
#7341 = CARTESIAN_POINT ( 'NONE',  ( -1.467888652719046449, -2.149340926099360782, 3.492485675378535603 ) ) ;
#7342 =( BOUNDED_CURVE ( )  B_SPLINE_CURVE ( 2, ( #4340, #6565, #2438, #8757, #800, #7967, #5070, #7316, #7878 ),
 .UNSPECIFIED., .F., .T. ) 
 B_SPLINE_CURVE_WITH_KNOTS ( ( 3, 2, 2, 2, 3 ),
 ( 0.2291666666666666574, 0.2361111111111111049, 0.2500000000000000000, 0.2638888888888888951, 0.2708333333333333703 ),
 .UNSPECIFIED. ) 
 CURVE ( )  GEOMETRIC_REPRESENTATION_ITEM ( )  RATIONAL_B_SPLINE_CURVE ( ( 0.9330127018922194093, 0.9330127018922194093, 1.000000000000000000, 0.8660254037844387076, 1.000000000000000000, 0.8660254037844387076, 1.000000000000000000, 0.9330127018922190762, 0.9330127018922194093 ) ) 
 REPRESENTATION_ITEM ( '' )  );
#7343 = CARTESIAN_POINT ( 'NONE',  ( 2.624999999999998668, -29.77083333265053611, -4.546633369868303021 ) ) ;
#7344 = DIRECTION ( 'NONE',  ( 0.000000000000000000, 0.000000000000000000, 1.000000000000000000 ) ) ;
#7345 = CARTESIAN_POINT ( 'NONE',  ( -5.385316468750000141, -28.07812499965860198, 0.000000000000000000 ) ) ;
#7346 = CARTESIAN_POINT ( 'NONE',  ( 1.674995433905601239, -2.949340926099360605, -3.992485675378532939 ) ) ;
#7347 = CARTESIAN_POINT ( 'NONE',  ( 0.000000000000000000, 0.000000000000000000, 0.000000000000000000 ) ) ;
#7348 = VERTEX_POINT ( 'NONE', #5616 ) ;
#7349 = CARTESIAN_POINT ( 'NONE',  ( -3.807688866302469071E-16, -28.14062499965860198, -6.218427825808274356 ) ) ;
#7350 = CARTESIAN_POINT ( 'NONE',  ( 1.260781871532430598, -3.450659073900639751, 2.992485675378564469 ) ) ;
#7351 = ORIENTED_EDGE ( 'NONE', *, *, #290, .T. ) ;
#7352 = CARTESIAN_POINT ( 'NONE',  ( 5.250000000000000000, -28.49999999999999645, 0.000000000000000000 ) ) ;
#7353 = DIRECTION ( 'NONE',  ( 0.000000000000000000, 0.000000000000000000, -1.000000000000000000 ) ) ;
#7354 = ADVANCED_FACE ( 'NONE', ( #7106 ), #8464, .T. ) ;
#7355 =( NAMED_UNIT ( * ) PLANE_ANGLE_UNIT ( ) SI_UNIT ( $, .RADIAN. ) );
#7356 = CARTESIAN_POINT ( 'NONE',  ( -5.250000000000000000, -27.75000000000000000, 0.000000000000000000 ) ) ;
#7357 = CARTESIAN_POINT ( 'NONE',  ( -5.250000000000000000, -30.18749999931720041, 0.000000000000000000 ) ) ;
#7358 = ADVANCED_FACE ( 'NONE', ( #8509 ), #7199, .F. ) ;
#7359 = CARTESIAN_POINT ( 'NONE',  ( -1.431606283892620235, -3.149340926099361671, -3.507514324621463953 ) ) ;
#7360 = DIRECTION ( 'NONE',  ( 0.000000000000000000, -0.000000000000000000, -1.000000000000000000 ) ) ;
#7361 = CARTESIAN_POINT ( 'NONE',  ( -2.624999999999998668, -27.44791666734946389, -4.546633369868303021 ) ) ;
#7362 = CARTESIAN_POINT ( 'NONE',  ( 5.114683531249998971, -28.94270833367473017, 2.952963913586936329 ) ) ;
#7363 = CARTESIAN_POINT ( 'NONE',  ( 0.000000000000000000, -28.00000000000000000, 0.000000000000000000 ) ) ;
#7364 = ORIENTED_EDGE ( 'NONE', *, *, #367, .T. ) ;
#7365 = CARTESIAN_POINT ( 'NONE',  ( -2.624999999999998668, -29.41666666666666785, -4.546633369868303021 ) ) ;
#7366 = CARTESIAN_POINT ( 'NONE',  ( 2.557341765625000818, -28.06770833367473017, -4.429445870380400052 ) ) ;
#7367 = ADVANCED_FACE ( 'NONE', ( #6402 ), #7902, .T. ) ;
#7368 = ORIENTED_EDGE ( 'NONE', *, *, #8333, .F. ) ;
#7369 = LINE ( 'NONE', #5736, #2138 ) ;
#7370 = CARTESIAN_POINT ( 'NONE',  ( -2.692658234375000514, -27.65104166632526628, -4.663820869356205989 ) ) ;
#7371 = CARTESIAN_POINT ( 'NONE',  ( -2.841254879263473310, -2.750659073900638685, -2.815599370228907716 ) ) ;
#7372 = CARTESIAN_POINT ( 'NONE',  ( 1.406733260263393293, -29.26116454900183328, -5.250000000000000000 ) ) ;
#7373 = CARTESIAN_POINT ( 'NONE',  ( 2.692658234374998738, -28.19270833299193413, -4.663820869356206877 ) ) ;
#7374 = VERTEX_POINT ( 'NONE', #2844 ) ;
#7375 = PLANE ( 'NONE',  #3274 ) ;
#7376 = CARTESIAN_POINT ( 'NONE',  ( -5.250000000000000888, -29.63541666734946389, 3.031088913245532979 ) ) ;
#7377 = CARTESIAN_POINT ( 'NONE',  ( -5.385316468750001029, -28.13020833299193058, -3.109213912904136734 ) ) ;
#7378 = CARTESIAN_POINT ( 'NONE',  ( 3.616337804771879580E-16, -27.29687500034139802, -5.905927827173866440 ) ) ;
#7379 = VERTEX_POINT ( 'NONE', #4997 ) ;
#7380 = DIRECTION ( 'NONE',  ( 1.000000000000000000, 0.000000000000000000, 0.000000000000000000 ) ) ;
#7381 = CARTESIAN_POINT ( 'NONE',  ( 3.007514324621436863, -0.4506590739006394175, 1.224499502706140719 ) ) ;
#7382 = DIRECTION ( 'NONE',  ( 0.000000000000000000, 1.000000000000000000, 0.000000000000000000 ) ) ;
#7383 = EDGE_CURVE ( 'NONE', #3793, #2600, #5477, .T. ) ;
#7384 =( GEOMETRIC_REPRESENTATION_CONTEXT ( 3 ) GLOBAL_UNCERTAINTY_ASSIGNED_CONTEXT ( ( #6539 ) ) GLOBAL_UNIT_ASSIGNED_CONTEXT ( ( #5818, #7170, #95 ) ) REPRESENTATION_CONTEXT ( 'NONE', 'WORKASPACE' ) );
#7385 = EDGE_CURVE ( 'NONE', #301, #8385, #5733, .T. ) ;
#7386 = CARTESIAN_POINT ( 'NONE',  ( -5.250000000000000000, -27.93749999931720396, 0.000000000000000000 ) ) ;
#7387 = DIRECTION ( 'NONE',  ( 0.000000000000000000, 0.000000000000000000, 1.000000000000000000 ) ) ;
#7388 = CARTESIAN_POINT ( 'NONE',  ( 2.487701488670255756, -1.249340926099361093, -2.462045979635577364 ) ) ;
#7389 = CARTESIAN_POINT ( 'NONE',  ( 5.250000000000000888, -29.08333333265053611, 3.031088913245533423 ) ) ;
#7390 = ORIENTED_EDGE ( 'NONE', *, *, #7742, .F. ) ;
#7391 = DIRECTION ( 'NONE',  ( 1.000000000000000000, 0.000000000000000000, 0.000000000000000000 ) ) ;
#7392 = COLOUR_RGB ( '',0.8941176470588234615, 0.8941176470588234615, 0.8941176470588234615 ) ;
#7393 = CARTESIAN_POINT ( 'NONE',  ( -2.692658234374996518, -28.53645833299193413, 4.663820869356208654 ) ) ;
#7394 = CARTESIAN_POINT ( 'NONE',  ( 1.638713065079161924, -3.949340926099361493, 4.007514324621467949 ) ) ;
#7395 = FACE_OUTER_BOUND ( 'NONE', #3612, .T. ) ;
#7396 = ORIENTED_EDGE ( 'NONE', *, *, #6506, .F. ) ;
#7397 = CARTESIAN_POINT ( 'NONE',  ( 5.385316468749999252, -28.18229166632526628, -3.109213912904139399 ) ) ;
#7398 = CARTESIAN_POINT ( 'NONE',  ( 0.01814118441313990887, -1.750659073900638907, 3.500000000000000000 ) ) ;
#7399 = ORIENTED_EDGE ( 'NONE', *, *, #9001, .F. ) ;
#7400 = CARTESIAN_POINT ( 'NONE',  ( -5.250000000000000000, -28.37499999999999645, -6.429395695523604153E-16 ) ) ;
#7401 =( BOUNDED_CURVE ( )  B_SPLINE_CURVE ( 2, ( #7643, #5499, #4109, #8346, #570, #1557, #7975, #1509, #6526 ),
 .UNSPECIFIED., .F., .T. ) 
 B_SPLINE_CURVE_WITH_KNOTS ( ( 3, 2, 2, 2, 3 ),
 ( 0.3541666666666666852, 0.3611111111111111049, 0.3750000000000000000, 0.3888888888888888951, 0.3958333333333333703 ),
 .UNSPECIFIED. ) 
 CURVE ( )  GEOMETRIC_REPRESENTATION_ITEM ( )  RATIONAL_B_SPLINE_CURVE ( ( 0.9330127018922194093, 0.9330127018922196314, 1.000000000000000000, 0.8660254037844387076, 1.000000000000000000, 0.8660254037844387076, 1.000000000000000000, 0.9330127018922190762, 0.9330127018922194093 ) ) 
 REPRESENTATION_ITEM ( '' )  );
#7402 = CARTESIAN_POINT ( 'NONE',  ( 2.487701488670203354, -0.3506590739006389956, 2.462045979635629323 ) ) ;
#7403 = ORIENTED_EDGE ( 'NONE', *, *, #430, .F. ) ;
#7404 = CARTESIAN_POINT ( 'NONE',  ( -5.250000000000000000, -27.27083333333333215, -3.031088913245534755 ) ) ;
#7405 = ORIENTED_EDGE ( 'NONE', *, *, #144, .T. ) ;
#7406 = AXIS2_PLACEMENT_3D ( 'NONE', #368, #1579, #231 ) ;
#7407 = CARTESIAN_POINT ( 'NONE',  ( 2.557341765624996821, -28.40104166700806587, 4.429445870380401828 ) ) ;
#7408 = CARTESIAN_POINT ( 'NONE',  ( -3.492485675378536047, -4.949340926099361049, -1.467888652719048670 ) ) ;
#7409 = DIRECTION ( 'NONE',  ( 0.000000000000000000, 1.000000000000000000, 0.000000000000000000 ) ) ;
#7410 = CARTESIAN_POINT ( 'NONE',  ( 0.000000000000000000, -27.00000000000000000, -5.250000000000000000 ) ) ;
#7411 = CARTESIAN_POINT ( 'NONE',  ( -5.114683531250000748, -28.54687500034139802, -6.263680815196995234E-16 ) ) ;
#7412 = CARTESIAN_POINT ( 'NONE',  ( 0.000000000000000000, 74.00000000000001421, -4.000000000000000000 ) ) ;
#7413 = EDGE_LOOP ( 'NONE', ( #2034, #4896, #2163, #7839 ) ) ;
#7414 = CARTESIAN_POINT ( 'NONE',  ( 1.406733260263391960, -29.30133545031537068, 5.250000000000000000 ) ) ;
#7415 = CARTESIAN_POINT ( 'NONE',  ( -2.557341765625002594, -26.94270833367473017, 4.429445870380399164 ) ) ;
#7416 = AXIS2_PLACEMENT_3D ( 'NONE', #6163, #4674, #8167 ) ;
#7417 = ORIENTED_EDGE ( 'NONE', *, *, #1329, .F. ) ;
#7418 = EDGE_CURVE ( 'NONE', #3705, #1374, #8085, .T. ) ;
#7419 = CARTESIAN_POINT ( 'NONE',  ( 0.000000000000000000, 81.00000000000001421, 0.000000000000000000 ) ) ;
#7420 = CARTESIAN_POINT ( 'NONE',  ( 1.142306659890740623E-15, -28.29687499965860553, 6.218427825808274356 ) ) ;
#7421 = CARTESIAN_POINT ( 'NONE',  ( 0.01814118441321938349, -1.449340926099360827, -4.000000000000000000 ) ) ;
#7422 = UNCERTAINTY_MEASURE_WITH_UNIT (LENGTH_MEASURE( 1.000000000000000082E-05 ), #3997, 'distance_accuracy_value', 'NONE');
#7423 =( NAMED_UNIT ( * ) PLANE_ANGLE_UNIT ( ) SI_UNIT ( $, .RADIAN. ) );
#7424 = CARTESIAN_POINT ( 'NONE',  ( 5.385316468750000141, -28.23437499965860198, -6.595110575850215044E-16 ) ) ;
#7425 = VERTEX_POINT ( 'NONE', #3903 ) ;
#7426 = CARTESIAN_POINT ( 'NONE',  ( 2.625000000000002220, -28.41666666666666785, 4.546633369868302132 ) ) ;
#7427 = CARTESIAN_POINT ( 'NONE',  ( -2.624999999999998668, -28.44791666734946389, -4.546633369868303021 ) ) ;
#7428 = CARTESIAN_POINT ( 'NONE',  ( 1.142306659890740623E-15, -28.54687499965860198, 6.218427825808274356 ) ) ;
#7429 = AXIS2_PLACEMENT_3D ( 'NONE', #5054, #2322, #2229 ) ;
#7430 = EDGE_CURVE ( 'NONE', #7863, #116, #8004, .T. ) ;
#7431 = ORIENTED_EDGE ( 'NONE', *, *, #3106, .T. ) ;
#7432 = CARTESIAN_POINT ( 'NONE',  ( -5.385316468749998364, -28.80729166632526272, 3.109213912904140287 ) ) ;
#7433 = CARTESIAN_POINT ( 'NONE',  ( 3.007514324621436863, -2.050659073900639839, 1.224499502706140719 ) ) ;
#7434 = DIRECTION ( 'NONE',  ( 0.000000000000000000, -1.000000000000000000, 0.000000000000000000 ) ) ;
#7435 = AXIS2_PLACEMENT_3D ( 'NONE', #2837, #7713, #4225 ) ;
#7436 = CARTESIAN_POINT ( 'NONE',  ( -3.712013335537174572E-16, -27.24999999931720041, -6.062177826491070398 ) ) ;
#7437 = CARTESIAN_POINT ( 'NONE',  ( -5.249999999999999112, -27.02083333333334281, -3.031088913245534755 ) ) ;
#7438 = CARTESIAN_POINT ( 'NONE',  ( -3.507514324621464397, -0.3493409260993610710, 1.431606283892619569 ) ) ;
#7439 = VECTOR ( 'NONE', #9070, 1000.000000000000000 ) ;
#7440 = CARTESIAN_POINT ( 'NONE',  ( 2.557341765625000818, -29.56770833367473017, -4.429445870380400052 ) ) ;
#7441 = ORIENTED_EDGE ( 'NONE', *, *, #2605, .T. ) ;
#7442 =( NAMED_UNIT ( * ) PLANE_ANGLE_UNIT ( ) SI_UNIT ( $, .RADIAN. ) );
#7443 = CARTESIAN_POINT ( 'NONE',  ( -5.385316468749998364, -28.30729166632526628, 3.109213912904140287 ) ) ;
#7444 = CARTESIAN_POINT ( 'NONE',  ( 3.992485675378533383, -2.549340926099360694, 1.674995433905599462 ) ) ;
#7445 = FACE_OUTER_BOUND ( 'NONE', #71, .T. ) ;
#7446 = ORIENTED_EDGE ( 'NONE', *, *, #5195, .F. ) ;
#7447 = CARTESIAN_POINT ( 'NONE',  ( -5.385316468750000141, -28.07812499965860198, 0.000000000000000000 ) ) ;
#7448 = CARTESIAN_POINT ( 'NONE',  ( 2.487701488670203354, -6.750659073900639129, 2.462045979635629323 ) ) ;
#7449 = ORIENTED_EDGE ( 'NONE', *, *, #933, .F. ) ;
#7450 = CARTESIAN_POINT ( 'NONE',  ( 3.712013335537174572E-16, -27.43750000000000000, -6.062177826491070398 ) ) ;
#7451 = CARTESIAN_POINT ( 'NONE',  ( 0.000000000000000000, -20.00000000000000000, -2.050090691792606279 ) ) ;
#7452 = CARTESIAN_POINT ( 'NONE',  ( -2.462045979635629323, -3.150659073900639040, 2.487701488670203798 ) ) ;
#7453 = ORIENTED_EDGE ( 'NONE', *, *, #7298, .F. ) ;
#7454 =( NAMED_UNIT ( * ) SI_UNIT ( $, .STERADIAN. ) SOLID_ANGLE_UNIT ( ) );
#7455 = CARTESIAN_POINT ( 'NONE',  ( -5.250000000000000000, -27.02083333333333570, -3.031088913245534755 ) ) ;
#7456 = EDGE_LOOP ( 'NONE', ( #6386, #4105 ) ) ;
#7457 = CARTESIAN_POINT ( 'NONE',  ( -5.114683531250000748, -29.23437500034139802, -6.263680815196995234E-16 ) ) ;
#7458 = CARTESIAN_POINT ( 'NONE',  ( 3.000000000000000444, -1.049340926099361582, 0.01814118441320859698 ) ) ;
#7459 = CARTESIAN_POINT ( 'NONE',  ( 2.300847884672513123E-14, -27.21875000068279959, -5.250000000000000000 ) ) ;
#7460 = CARTESIAN_POINT ( 'NONE',  ( 5.114683531249999859, -28.65104166700806587, -2.952963913586932776 ) ) ;
#7461 = DIRECTION ( 'NONE',  ( 0.000000000000000000, -1.000000000000000000, 0.000000000000000000 ) ) ;
#7462 = EDGE_CURVE ( 'NONE', #1378, #4147, #5015, .T. ) ;
#7463 = CARTESIAN_POINT ( 'NONE',  ( -2.324088772396477476E-15, -29.46875000068279959, -5.250000000000000000 ) ) ;
#7464 = CARTESIAN_POINT ( 'NONE',  ( 5.114683531250000748, -26.85937500034139802, 0.000000000000000000 ) ) ;
#7465 = EDGE_LOOP ( 'NONE', ( #6901, #1576 ) ) ;
#7466 = LINE ( 'NONE', #8260, #4000 ) ;
#7467 = CARTESIAN_POINT ( 'NONE',  ( 2.692658234374998738, -29.19270833299193413, -4.663820869356206877 ) ) ;
#7468 = CIRCLE ( 'NONE', #5086, 5.250000000000000000 ) ;
#7469 = DIRECTION ( 'NONE',  ( -0.000000000000000000, 1.000000000000000000, -0.000000000000000000 ) ) ;
#7470 = CARTESIAN_POINT ( 'NONE',  ( 5.385316468750000141, -29.48437499965859843, -6.595110575850215044E-16 ) ) ;
#7471 = VERTEX_POINT ( 'NONE', #8731 ) ;
#7472 = DIRECTION ( 'NONE',  ( 0.000000000000000000, -0.000000000000000000, -1.000000000000000000 ) ) ;
#7473 = CARTESIAN_POINT ( 'NONE',  ( -2.625000000000002220, -27.86458333401612819, 4.546633369868302132 ) ) ;
#7474 = CARTESIAN_POINT ( 'NONE',  ( -2.692658234374996518, -29.31770833299193413, 4.663820869356208654 ) ) ;
#7475 = UNCERTAINTY_MEASURE_WITH_UNIT (LENGTH_MEASURE( 1.000000000000000082E-05 ), #7774, 'distance_accuracy_value', 'NONE');
#7476 = ORIENTED_EDGE ( 'NONE', *, *, #367, .F. ) ;
#7477 = CARTESIAN_POINT ( 'NONE',  ( -3.807688866302469071E-16, -27.89062499965860198, -6.218427825808274356 ) ) ;
#7478 = CARTESIAN_POINT ( 'NONE',  ( -1.467888652718973619, -1.050659073900638951, -3.492485675378565801 ) ) ;
#7479 = DIRECTION ( 'NONE',  ( 0.000000000000000000, 1.000000000000000000, 0.000000000000000000 ) ) ;
#7480 = VECTOR ( 'NONE', #2273, 1000.000000000000000 ) ;
#7481 =( BOUNDED_CURVE ( )  B_SPLINE_CURVE ( 2, ( #4634, #4772, #6021, #8950, #3342, #9045, #7426, #5418, #8858 ),
 .UNSPECIFIED., .F., .T. ) 
 B_SPLINE_CURVE_WITH_KNOTS ( ( 3, 2, 2, 2, 3 ),
 ( 0.4375000000000000000, 0.4444444444444444198, 0.4583333333333333148, 0.4722222222222222099, 0.4791666666666666852 ),
 .UNSPECIFIED. ) 
 CURVE ( )  GEOMETRIC_REPRESENTATION_ITEM ( )  RATIONAL_B_SPLINE_CURVE ( ( 0.9330127018922194093, 0.9330127018922194093, 1.000000000000000000, 0.8660254037844387076, 1.000000000000000000, 0.8660254037844387076, 1.000000000000000000, 0.9330127018922190762, 0.9330127018922194093 ) ) 
 REPRESENTATION_ITEM ( '' )  );
#7482 = CIRCLE ( 'NONE', #3767, 2.999999999999999556 ) ;
#7483 = CARTESIAN_POINT ( 'NONE',  ( -5.249999999999999112, -28.89583333333333215, -3.031088913245536975 ) ) ;
#7484 = DIRECTION ( 'NONE',  ( 0.000000000000000000, 0.000000000000000000, 1.000000000000000000 ) ) ;
#7485 = CARTESIAN_POINT ( 'NONE',  ( 2.625000000000000444, -27.98958333401612819, -4.546633369868303021 ) ) ;
#7486 = ADVANCED_FACE ( 'NONE', ( #4550 ), #3857, .F. ) ;
#7487 = DIRECTION ( 'NONE',  ( 0.000000000000000000, 0.000000000000000000, -1.000000000000000000 ) ) ;
#7488 = CARTESIAN_POINT ( 'NONE',  ( 5.249999999999999112, -27.72916666666666430, -3.031088913245534755 ) ) ;
#7489 = SHAPE_DEFINITION_REPRESENTATION ( #8825, #1697 ) ;
#7490 = CARTESIAN_POINT ( 'NONE',  ( 5.385316468749999252, -29.93229166632526983, -3.109213912904139399 ) ) ;
#7491 = CARTESIAN_POINT ( 'NONE',  ( 2.108492589042307408, -0.8493409260993616261, 2.134148098076978251 ) ) ;
#7492 = CIRCLE ( 'NONE', #4943, 2.629341307491595447 ) ;
#7493 = FACE_OUTER_BOUND ( 'NONE', #1453, .T. ) ;
#7494 = CARTESIAN_POINT ( 'NONE',  ( -3.807688866302469071E-16, -28.39062499965859843, -6.218427825808274356 ) ) ;
#7495 = CARTESIAN_POINT ( 'NONE',  ( -3.492485675378566246, -6.250659073900641793, 1.467888652718973397 ) ) ;
#7496 = VERTEX_POINT ( 'NONE', #3162 ) ;
#7497 = CARTESIAN_POINT ( 'NONE',  ( 5.250000000000000000, -27.99999999999999645, 0.000000000000000000 ) ) ;
#7498 = DIRECTION ( 'NONE',  ( 0.000000000000000000, -1.000000000000000000, 0.000000000000000000 ) ) ;
#7499 = CARTESIAN_POINT ( 'NONE',  ( 0.01814118441313990887, -1.750659073900638907, 3.500000000000000000 ) ) ;
#7500 = EDGE_LOOP ( 'NONE', ( #2457, #6556, #7521, #1193 ) ) ;
#7501 = CARTESIAN_POINT ( 'NONE',  ( -5.250000000000000000, -28.27083333333332860, -3.031088913245534755 ) ) ;
#7502 = ORIENTED_EDGE ( 'NONE', *, *, #435, .F. ) ;
#7503 = CARTESIAN_POINT ( 'NONE',  ( 5.114683531250000748, -28.33854166700806587, -2.952963913586932776 ) ) ;
#7504 = CARTESIAN_POINT ( 'NONE',  ( -1.224499502706077880, -3.149340926099362115, -3.007514324621463064 ) ) ;
#7505 = DIRECTION ( 'NONE',  ( 0.000000000000000000, 0.000000000000000000, -1.000000000000000000 ) ) ;
#7506 = CYLINDRICAL_SURFACE ( 'NONE', #7169, 5.250000000000000000 ) ;
#7507 = CARTESIAN_POINT ( 'NONE',  ( -1.084901341431563923E-15, -28.73437500034139802, 5.905927827173866440 ) ) ;
#7508 = FILL_AREA_STYLE_COLOUR ( '', #6579 ) ;
#7509 = CYLINDRICAL_SURFACE ( 'NONE', #2548, 5.250000000000000000 ) ;
#7510 = ORIENTED_EDGE ( 'NONE', *, *, #2944, .T. ) ;
#7511 = DIRECTION ( 'NONE',  ( -0.000000000000000000, -1.000000000000000000, -0.000000000000000000 ) ) ;
#7512 = CARTESIAN_POINT ( 'NONE',  ( -2.692658234375000514, -28.65104166632526628, -4.663820869356205989 ) ) ;
#7513 = CARTESIAN_POINT ( 'NONE',  ( -5.385316468749998364, -29.83854166632526983, 3.109213912904140287 ) ) ;
#7514 = DIRECTION ( 'NONE',  ( 0.000000000000000000, 1.000000000000000000, 0.000000000000000000 ) ) ;
#7515 = CARTESIAN_POINT ( 'NONE',  ( 5.385316468750000141, -28.73437499965860198, -6.595110575850215044E-16 ) ) ;
#7516 = CARTESIAN_POINT ( 'NONE',  ( 2.815599370228847320, -7.249340926099360871, 2.841254879263533262 ) ) ;
#7517 = ORIENTED_EDGE ( 'NONE', *, *, #2193, .T. ) ;
#7518 = CARTESIAN_POINT ( 'NONE',  ( 1.975475456537005874E-15, -27.43750000000000000, 5.250000000000000000 ) ) ;
#7519 = CARTESIAN_POINT ( 'NONE',  ( -5.250000000000000000, -28.15625000068279604, -6.429395695523604153E-16 ) ) ;
#7520 = CARTESIAN_POINT ( 'NONE',  ( -5.385316468749998364, -29.33854166632526983, 3.109213912904140287 ) ) ;
#7521 = ORIENTED_EDGE ( 'NONE', *, *, #4460, .F. ) ;
#7522 = CARTESIAN_POINT ( 'NONE',  ( -2.692658234375000514, -28.86979166632526983, -4.663820869356205989 ) ) ;
#7523 = CARTESIAN_POINT ( 'NONE',  ( 1.467888652718972731, -0.2506590739006389068, 3.492485675378566246 ) ) ;
#7524 = CARTESIAN_POINT ( 'NONE',  ( 0.000000000000000000, 75.00000000000000000, 0.000000000000000000 ) ) ;
#7525 = EDGE_CURVE ( 'NONE', #8002, #1439, #5239, .T. ) ;
#7526 = SURFACE_STYLE_USAGE ( .BOTH. , #1811 ) ;
#7527 = CARTESIAN_POINT ( 'NONE',  ( 2.625000000000000444, -28.20833333333333215, -4.546633369868303021 ) ) ;
#7528 = DIRECTION ( 'NONE',  ( 0.000000000000000000, -1.000000000000000000, 0.000000000000000000 ) ) ;
#7529 = DIRECTION ( 'NONE',  ( 0.000000000000000000, 0.000000000000000000, 1.000000000000000000 ) ) ;
#7530 = ORIENTED_EDGE ( 'NONE', *, *, #3908, .T. ) ;
#7531 = PRODUCT_CONTEXT ( 'NONE', #2733, 'mechanical' ) ;
#7532 = CARTESIAN_POINT ( 'NONE',  ( -5.385316468750000141, -29.32812499965859843, 0.000000000000000000 ) ) ;
#7533 = CARTESIAN_POINT ( 'NONE',  ( 3.007514324621463508, -1.149340926099361448, -1.224499502706076770 ) ) ;
#7534 = EDGE_CURVE ( 'NONE', #4663, #1286, #5939, .T. ) ;
#7535 = CARTESIAN_POINT ( 'NONE',  ( 0.000000000000000000, -30.00000000000000000, 0.000000000000000000 ) ) ;
#7536 =( BOUNDED_CURVE ( )  B_SPLINE_CURVE ( 2, ( #3706, #8124, #7940, #3107, #7283, #5088, #164, #3656, #6673 ),
 .UNSPECIFIED., .F., .T. ) 
 B_SPLINE_CURVE_WITH_KNOTS ( ( 3, 2, 2, 2, 3 ),
 ( 0.2291666666666666574, 0.2361111111111111049, 0.2500000000000000000, 0.2638888888888888951, 0.2708333333333333703 ),
 .UNSPECIFIED. ) 
 CURVE ( )  GEOMETRIC_REPRESENTATION_ITEM ( )  RATIONAL_B_SPLINE_CURVE ( ( 0.9330127018922194093, 0.9330127018922194093, 1.000000000000000000, 0.8660254037844387076, 1.000000000000000000, 0.8660254037844387076, 1.000000000000000000, 0.9330127018922190762, 0.9330127018922194093 ) ) 
 REPRESENTATION_ITEM ( '' )  );
#7537 = CARTESIAN_POINT ( 'NONE',  ( 5.385316468750000141, -28.95312499965860198, -6.595110575850215044E-16 ) ) ;
#7538 = CARTESIAN_POINT ( 'NONE',  ( 2.462045979635629767, -2.350659073900639218, -2.487701488670203354 ) ) ;
#7539 = EDGE_LOOP ( 'NONE', ( #5391, #1623 ) ) ;
#7540 = CARTESIAN_POINT ( 'NONE',  ( 6.429395695523604153E-16, -30.00000000000000000, -5.250000000000000000 ) ) ;
#7541 = DIRECTION ( 'NONE',  ( 0.000000000000000000, 1.000000000000000000, 0.000000000000000000 ) ) ;
#7542 = CARTESIAN_POINT ( 'NONE',  ( -5.250000000000000000, -30.18749999931720041, 0.000000000000000000 ) ) ;
#7543 = PRESENTATION_LAYER_ASSIGNMENT (  '', '', ( #2340 ) ) ;
#7544 = ORIENTED_EDGE ( 'NONE', *, *, #3669, .F. ) ;
#7545 = SURFACE_STYLE_USAGE ( .BOTH. , #2762 ) ;
#7546 = CARTESIAN_POINT ( 'NONE',  ( 2.624999999999998668, -29.08333333333333215, -4.546633369868303021 ) ) ;
#7547 = ORIENTED_EDGE ( 'NONE', *, *, #3479, .F. ) ;
#7548 = CARTESIAN_POINT ( 'NONE',  ( -1.084901341431563726E-15, -28.67187500034139802, 5.905927827173866440 ) ) ;
#7549 = CARTESIAN_POINT ( 'NONE',  ( 3.007514324621463508, -4.349340926099361404, -1.224499502706076770 ) ) ;
#7550 = CARTESIAN_POINT ( 'NONE',  ( -1.406733260263385521, -28.07366454968462932, 5.250000000000006217 ) ) ;
#7551 = CARTESIAN_POINT ( 'NONE',  ( 2.557341765624996821, -27.46354166700806587, 4.429445870380401828 ) ) ;
#7552 = AXIS2_PLACEMENT_3D ( 'NONE', #3816, #2371, #5201 ) ;
#7553 = DIRECTION ( 'NONE',  ( 0.000000000000000000, 1.000000000000000000, 0.000000000000000000 ) ) ;
#7554 = CARTESIAN_POINT ( 'NONE',  ( -2.752888856892141689, -2.800711225422160581E-13, 1.838534025203911515 ) ) ;
#7555 = CARTESIAN_POINT ( 'NONE',  ( -5.114683531250000748, -27.46354166700806232, 2.952963913586931888 ) ) ;
#7556 =( NAMED_UNIT ( * ) SI_UNIT ( $, .STERADIAN. ) SOLID_ANGLE_UNIT ( ) );
#7557 = CARTESIAN_POINT ( 'NONE',  ( -5.114683531249999859, -28.81770833367473017, -2.952963913586935440 ) ) ;
#7558 = DIRECTION ( 'NONE',  ( 0.000000000000000000, 1.000000000000000000, 0.000000000000000000 ) ) ;
#7559 = CARTESIAN_POINT ( 'NONE',  ( -5.385316468749998364, -28.58854166632526628, 3.109213912904140287 ) ) ;
#7560 = ADVANCED_FACE ( 'NONE', ( #1615 ), #1060, .F. ) ;
#7561 = CARTESIAN_POINT ( 'NONE',  ( -5.249999999999999112, -28.64583333333332860, -3.031088913245536975 ) ) ;
#7562 = CARTESIAN_POINT ( 'NONE',  ( 6.429395695523604153E-16, -30.00000000000000000, -5.250000000000000000 ) ) ;
#7563 = CARTESIAN_POINT ( 'NONE',  ( -2.692658234374996518, -29.31770833299193413, 4.663820869356208654 ) ) ;
#7564 = CARTESIAN_POINT ( 'NONE',  ( 1.431606283892619125, -0.7493409260993610932, 3.507514324621464397 ) ) ;
#7565 = ORIENTED_EDGE ( 'NONE', *, *, #5260, .T. ) ;
#7566 = CIRCLE ( 'NONE', #8747, 2.999999999999999556 ) ;
#7567 = CARTESIAN_POINT ( 'NONE',  ( -2.624999999999996891, -27.45833333333333570, 4.546633369868304797 ) ) ;
#7568 = CARTESIAN_POINT ( 'NONE',  ( -2.625000000000002220, -27.36458333401612819, 4.546633369868302132 ) ) ;
#7569 = CARTESIAN_POINT ( 'NONE',  ( 5.385316468750000141, -28.73437499965860198, -6.595110575850215044E-16 ) ) ;
#7570 = VERTEX_POINT ( 'NONE', #310 ) ;
#7571 = AXIS2_PLACEMENT_3D ( 'NONE', #4089, #6222, #1995 ) ;
#7572 = CARTESIAN_POINT ( 'NONE',  ( 5.385316468749999252, -28.43229166632526272, -3.109213912904138954 ) ) ;
#7573 = CARTESIAN_POINT ( 'NONE',  ( -2.462045979635629323, -3.150659073900639040, 2.487701488670203798 ) ) ;
#7574 = DIRECTION ( 'NONE',  ( 0.000000000000000000, -1.000000000000000000, 0.000000000000000000 ) ) ;
#7575 = PRODUCT_DEFINITION_SHAPE ( 'NONE', 'NONE',  #9195 ) ;
#7576 = EDGE_CURVE ( 'NONE', #803, #7933, #2409, .T. ) ;
#7577 = CARTESIAN_POINT ( 'NONE',  ( -5.250000000000000888, -28.85416666666667140, 3.031088913245533423 ) ) ;
#7578 = LINE ( 'NONE', #6028, #2879 ) ;
#7579 = AXIS2_PLACEMENT_3D ( 'NONE', #7744, #1367, #6997 ) ;
#7580 = CARTESIAN_POINT ( 'NONE',  ( 2.300847884672513123E-14, -27.96875000068279959, -5.250000000000000000 ) ) ;
#7581 = CARTESIAN_POINT ( 'NONE',  ( -1.975475456537005874E-15, -27.34375000068279249, 5.249999999999999112 ) ) ;
#7582 = CARTESIAN_POINT ( 'NONE',  ( 1.975475456537005874E-15, -27.37499999931720041, 5.249999999999999112 ) ) ;
#7583 = AXIS2_PLACEMENT_3D ( 'NONE', #6068, #350, #8904 ) ;
#7584 = ITEM_DEFINED_TRANSFORMATION ( 'NONE', 'NONE', #4130,  #888 ) ;
#7585 = CARTESIAN_POINT ( 'NONE',  ( -5.385316468750000141, -30.07812499965859843, 0.000000000000000000 ) ) ;
#7586 = CARTESIAN_POINT ( 'NONE',  ( -3.507514324621464397, -6.749340926099361759, 1.431606283892619347 ) ) ;
#7587 = CARTESIAN_POINT ( 'NONE',  ( -5.249999999999997335, -27.97916666666666430, 3.031088913245538308 ) ) ;
#7588 = CARTESIAN_POINT ( 'NONE',  ( 5.385316468750000141, -29.45312499965859843, -6.595110575850215044E-16 ) ) ;
#7589 = CARTESIAN_POINT ( 'NONE',  ( -3.500000000000000000, -4.550659073900638951, 0.01814118441314012051 ) ) ;
#7590 = ORIENTED_EDGE ( 'NONE', *, *, #358, .F. ) ;
#7591 = CARTESIAN_POINT ( 'NONE',  ( 6.429395695523604153E-16, -30.00000000000000000, -5.250000000000000000 ) ) ;
#7592 = AXIS2_PLACEMENT_3D ( 'NONE', #4962, #5053, #690 ) ;
#7593 = CARTESIAN_POINT ( 'NONE',  ( 0.000000000000000000, -20.00000000000000000, 0.000000000000000000 ) ) ;
#7594 = CARTESIAN_POINT ( 'NONE',  ( -3.500000000000000000, -4.550659073900638951, 0.01814118441314012051 ) ) ;
#7595 = ORIENTED_EDGE ( 'NONE', *, *, #783, .T. ) ;
#7596 = CARTESIAN_POINT ( 'NONE',  ( 2.624999999999998668, -28.83333333333333215, -4.546633369868303021 ) ) ;
#7597 = VECTOR ( 'NONE', #2250, 1000.000000000000000 ) ;
#7598 = ORIENTED_EDGE ( 'NONE', *, *, #6449, .T. ) ;
#7599 = CARTESIAN_POINT ( 'NONE',  ( 5.114683531250000748, -27.85937500034139802, 0.000000000000000000 ) ) ;
#7600 = CARTESIAN_POINT ( 'NONE',  ( 2.108492589042307408, -4.049340926099361582, 2.134148098076978251 ) ) ;
#7601 = DIRECTION ( 'NONE',  ( 0.000000000000000000, 0.000000000000000000, -1.000000000000000000 ) ) ;
#7602 = CARTESIAN_POINT ( 'NONE',  ( -5.114683531250000748, -27.77604166700806587, 2.952963913586931888 ) ) ;
#7603 = FACE_OUTER_BOUND ( 'NONE', #8980, .T. ) ;
#7604 = CARTESIAN_POINT ( 'NONE',  ( 6.429395695523604153E-16, -30.00000000000000000, -5.250000000000000000 ) ) ;
#7605 = CYLINDRICAL_SURFACE ( 'NONE', #6525, 4.250000000000000000 ) ;
#7606 = EDGE_CURVE ( 'NONE', #7933, #7374, #5625, .T. ) ;
#7607 = CARTESIAN_POINT ( 'NONE',  ( 5.114683531250000748, -29.17187500034139802, 0.000000000000000000 ) ) ;
#7608 = CARTESIAN_POINT ( 'NONE',  ( 1.045839947578414884E-14, -27.81249999999999289, -5.250000000000000000 ) ) ;
#7609 = CARTESIAN_POINT ( 'NONE',  ( -3.807688866302469071E-16, -28.42187499965860198, -6.218427825808274356 ) ) ;
#7610 = CARTESIAN_POINT ( 'NONE',  ( 1.142306659890740623E-15, -29.54687499965859487, 6.218427825808274356 ) ) ;
#7611 = CARTESIAN_POINT ( 'NONE',  ( 0.000000000000000000, -30.00000000000000000, 0.000000000000000000 ) ) ;
#7612 = CARTESIAN_POINT ( 'NONE',  ( -5.385316468750001029, -28.88020833299193768, -3.109213912904136734 ) ) ;
#7613 = CARTESIAN_POINT ( 'NONE',  ( -1.431606283892620235, -3.149340926099361671, -3.507514324621463953 ) ) ;
#7614 = CARTESIAN_POINT ( 'NONE',  ( 1.674995433905601239, -6.149340926099362115, -3.992485675378532939 ) ) ;
#7615 = ORIENTED_EDGE ( 'NONE', *, *, #3389, .T. ) ;
#7616 = CARTESIAN_POINT ( 'NONE',  ( 5.250000000000000000, -29.28125000068279604, 0.000000000000000000 ) ) ;
#7617 = CARTESIAN_POINT ( 'NONE',  ( -5.250000000000000888, -28.13541666734947100, 3.031088913245532979 ) ) ;
#7618 = CARTESIAN_POINT ( 'NONE',  ( -3.807688866302469071E-16, -28.67187499965860198, -6.218427825808274356 ) ) ;
#7619 = ORIENTED_EDGE ( 'NONE', *, *, #5310, .T. ) ;
#7620 = CARTESIAN_POINT ( 'NONE',  ( 5.385316468750001029, -27.72395833299193413, 3.109213912904134958 ) ) ;
#7621 = CARTESIAN_POINT ( 'NONE',  ( -0.01814118441314477650, -7.350659073900640550, -3.000000000000000444 ) ) ;
#7622 = DIRECTION ( 'NONE',  ( 0.000000000000000000, 0.000000000000000000, 1.000000000000000000 ) ) ;
#7623 = CARTESIAN_POINT ( 'NONE',  ( 1.406733260263405061, -28.19866454968462577, -5.249999999999994671 ) ) ;
#7624 = CARTESIAN_POINT ( 'NONE',  ( -3.500000000000000000, -8.249340926099360871, -0.01814118441321344033 ) ) ;
#7625 = AXIS2_PLACEMENT_3D ( 'NONE', #6420, #8487, #7082 ) ;
#7626 = CARTESIAN_POINT ( 'NONE',  ( -2.557341765625002594, -29.69270833367473017, 4.429445870380399164 ) ) ;
#7627 = DIRECTION ( 'NONE',  ( 0.000000000000000000, 1.000000000000000000, 0.000000000000000000 ) ) ;
#7628 = ITEM_DEFINED_TRANSFORMATION ( 'NONE', 'NONE', #8732,  #888 ) ;
#7629 = CARTESIAN_POINT ( 'NONE',  ( 2.692658234374998738, -28.91145833299193413, -4.663820869356206877 ) ) ;
#7630 = CARTESIAN_POINT ( 'NONE',  ( -2.462045979635576920, -4.849340926099361404, -2.487701488670255756 ) ) ;
#7631 = CARTESIAN_POINT ( 'NONE',  ( -6.972266317189433020E-16, -28.49999999931720041, -5.250000000000000000 ) ) ;
#7632 = AXIS2_PLACEMENT_3D ( 'NONE', #9012, #7627, #1256 ) ;
#7633 = CARTESIAN_POINT ( 'NONE',  ( 2.692658234374998738, -27.19270833299193413, -4.663820869356206877 ) ) ;
#7634 = CARTESIAN_POINT ( 'NONE',  ( 2.841254879263473310, -3.550659073900638063, 2.815599370228907272 ) ) ;
#7635 = CYLINDRICAL_SURFACE ( 'NONE', #785, 5.250000000000000000 ) ;
#7636 = DIRECTION ( 'NONE',  ( 0.000000000000000000, 1.000000000000000000, 0.000000000000000000 ) ) ;
#7637 = AXIS2_PLACEMENT_3D ( 'NONE', #5937, #5797, #3807 ) ;
#7638 = ORIENTED_EDGE ( 'NONE', *, *, #8052, .T. ) ;
#7639 = PRESENTATION_STYLE_ASSIGNMENT (( #2012 ) ) ;
#7640 = CARTESIAN_POINT ( 'NONE',  ( 5.250000000000000000, -28.37500000000000000, -6.429395695523604153E-16 ) ) ;
#7641 = CARTESIAN_POINT ( 'NONE',  ( 5.114683531249998971, -28.13020833367473017, 2.952963913586936329 ) ) ;
#7642 = CARTESIAN_POINT ( 'NONE',  ( -0.01814118441320841310, -3.849340926099361404, 3.000000000000000444 ) ) ;
#7643 = CARTESIAN_POINT ( 'NONE',  ( 1.045839947578414884E-14, -28.06249999999999289, -5.250000000000000000 ) ) ;
#7644 = CARTESIAN_POINT ( 'NONE',  ( -5.114683531250000748, -27.27604166700806232, 2.952963913586931888 ) ) ;
#7645 = CARTESIAN_POINT ( 'NONE',  ( 0.000000000000000000, -27.00000000000000000, 0.000000000000000000 ) ) ;
#7646 = EDGE_CURVE ( 'NONE', #8929, #5643, #5325, .T. ) ;
#7647 = CARTESIAN_POINT ( 'NONE',  ( -2.557341765624999042, -29.33854166700806232, -4.429445870380400052 ) ) ;
#7648 = PRODUCT_DEFINITION_SHAPE ( 'NONE', 'NONE',  #9191 ) ;
#7649 = CARTESIAN_POINT ( 'NONE',  ( -1.406733260263382856, -28.42633545031537068, -5.250000000000006217 ) ) ;
#7650 = CARTESIAN_POINT ( 'NONE',  ( 5.114683531249998971, -28.69270833367473017, 2.952963913586936329 ) ) ;
#7651 =( BOUNDED_CURVE ( )  B_SPLINE_CURVE ( 2, ( #7994, #7204, #829, #6684, #1622, #7389, #8737, #1013, #2981 ),
 .UNSPECIFIED., .F., .F. ) 
 B_SPLINE_CURVE_WITH_KNOTS ( ( 3, 2, 2, 2, 3 ),
 ( 0.6041666666666667407, 0.6111111111111111605, 0.6250000000000000000, 0.6388888888888888395, 0.6458333333333333703 ),
 .UNSPECIFIED. ) 
 CURVE ( )  GEOMETRIC_REPRESENTATION_ITEM ( )  RATIONAL_B_SPLINE_CURVE ( ( 0.9330127018922192983, 0.9330127018922198534, 1.000000000000000000, 0.8660254037844387076, 1.000000000000000000, 0.8660254037844387076, 1.000000000000000000, 0.9330127018922187432, 0.9330127018922192983 ) ) 
 REPRESENTATION_ITEM ( '' )  );
#7652 = EDGE_CURVE ( 'NONE', #3243, #2470, #685, .T. ) ;
#7653 = FACE_OUTER_BOUND ( 'NONE', #2615, .T. ) ;
#7654 = CARTESIAN_POINT ( 'NONE',  ( -5.249999999999999112, -29.41666666598387181, 3.031088913245538308 ) ) ;
#7655 = CARTESIAN_POINT ( 'NONE',  ( 5.385316468750001029, -29.75520833299193413, 3.109213912904134958 ) ) ;
#7656 = DIRECTION ( 'NONE',  ( 1.000000000000000000, 0.000000000000000000, 0.000000000000000000 ) ) ;
#7657 = CARTESIAN_POINT ( 'NONE',  ( -3.807688866302469071E-16, -29.17187499965859843, -6.218427825808274356 ) ) ;
#7658 = CARTESIAN_POINT ( 'NONE',  ( -3.492485675378536047, -1.749340926099361093, -1.467888652719048670 ) ) ;
#7659 = CARTESIAN_POINT ( 'NONE',  ( -1.638713065079163034, -7.949340926099362825, -4.007514324621466173 ) ) ;
#7660 = ORIENTED_EDGE ( 'NONE', *, *, #8818, .F. ) ;
#7661 =( REPRESENTATION_RELATIONSHIP ('NONE','NONE', #735, #3200 ) REPRESENTATION_RELATIONSHIP_WITH_TRANSFORMATION ( #1912 )SHAPE_REPRESENTATION_RELATIONSHIP( ) );
#7662 = CARTESIAN_POINT ( 'NONE',  ( -1.113604000661152470E-15, -26.84375000068279959, 6.062177826491070398 ) ) ;
#7663 = CARTESIAN_POINT ( 'NONE',  ( -3.807688866302469071E-16, -29.17187499965859843, -6.218427825808274356 ) ) ;
#7664 = ORIENTED_EDGE ( 'NONE', *, *, #1464, .T. ) ;
#7665 = CARTESIAN_POINT ( 'NONE',  ( -5.385316468750000141, -29.82812499965859843, 0.000000000000000000 ) ) ;
#7666 = CARTESIAN_POINT ( 'NONE',  ( -2.992485675378564469, -6.250659073900639129, 1.260781871532430820 ) ) ;
#7667 = CARTESIAN_POINT ( 'NONE',  ( 0.000000000000000000, -27.00000000000000000, 0.000000000000000000 ) ) ;
#7668 = PLANE ( 'NONE',  #4473 ) ;
#7669 = DIRECTION ( 'NONE',  ( 0.000000000000000000, 0.000000000000000000, -1.000000000000000000 ) ) ;
#7670 = CYLINDRICAL_SURFACE ( 'NONE', #5788, 5.250000000000000000 ) ;
#7671 = CARTESIAN_POINT ( 'NONE',  ( 3.616337804771879580E-16, -28.04687500034139802, -5.905927827173866440 ) ) ;
#7672 = FACE_OUTER_BOUND ( 'NONE', #2068, .T. ) ;
#7673 = APPLICATION_PROTOCOL_DEFINITION ( 'draft international standard', 'automotive_design', 1998, #8129 ) ;
#7674 = CARTESIAN_POINT ( 'NONE',  ( -2.692658234374996518, -29.78645833299193413, 4.663820869356208654 ) ) ;
#7675 = ADVANCED_FACE ( 'NONE', ( #3023 ), #5846, .F. ) ;
#7676 = CARTESIAN_POINT ( 'NONE',  ( -2.462045979635576920, -3.249340926099361315, -2.487701488670255756 ) ) ;
#7677 = CARTESIAN_POINT ( 'NONE',  ( 5.250000000000000888, -28.58333333265053611, 3.031088913245533423 ) ) ;
#7678 = CARTESIAN_POINT ( 'NONE',  ( -5.385316468749998364, -27.33854166632526628, 3.109213912904140287 ) ) ;
#7679 = CARTESIAN_POINT ( 'NONE',  ( -4.007514324621431534, -6.050659073900639839, -1.638713065079248521 ) ) ;
#7680 = CARTESIAN_POINT ( 'NONE',  ( -5.250000000000000888, -27.13541666734946389, 3.031088913245533423 ) ) ;
#7681 = CARTESIAN_POINT ( 'NONE',  ( 0.000000000000000000, 70.00000000000000000, -3.000000000000000444 ) ) ;
#7682 = ORIENTED_EDGE ( 'NONE', *, *, #5379, .T. ) ;
#7683 = CARTESIAN_POINT ( 'NONE',  ( 1.113604000661152470E-15, -28.68750000000000000, 6.062177826491070398 ) ) ;
#7684 = CARTESIAN_POINT ( 'NONE',  ( 2.557341765625000818, -27.81770833367473017, -4.429445870380400052 ) ) ;
#7685 = CARTESIAN_POINT ( 'NONE',  ( 3.007514324621436863, -0.4506590739006394175, 1.224499502706140719 ) ) ;
#7686 = CARTESIAN_POINT ( 'NONE',  ( -5.114683531250000748, -27.04687500034139802, -6.263680815196995234E-16 ) ) ;
#7687 = DIRECTION ( 'NONE',  ( 0.000000000000000000, 0.000000000000000000, -1.000000000000000000 ) ) ;
#7688 = MECHANICAL_DESIGN_GEOMETRIC_PRESENTATION_REPRESENTATION (  '', ( #3826 ), #2798 ) ;
#7689 = CARTESIAN_POINT ( 'NONE',  ( 5.114683531249998971, -29.44270833367473372, 2.952963913586936329 ) ) ;
#7690 = DIRECTION ( 'NONE',  ( 0.000000000000000000, 1.000000000000000000, 0.000000000000000000 ) ) ;
#7691 = CARTESIAN_POINT ( 'NONE',  ( 5.114683531249998971, -29.69270833367473017, 2.952963913586936329 ) ) ;
#7692 = STYLED_ITEM ( 'NONE', ( #1719 ), #2538 ) ;
#7693 = DIRECTION ( 'NONE',  ( 0.000000000000000000, -1.000000000000000000, 0.000000000000000000 ) ) ;
#7694 = CARTESIAN_POINT ( 'NONE',  ( 5.250000000000000000, -29.06249999931720396, -6.429395695523604153E-16 ) ) ;
#7695 = SURFACE_STYLE_FILL_AREA ( #581 ) ;
#7696 = CARTESIAN_POINT ( 'NONE',  ( -2.625000000000000444, -27.22916666598386826, -4.546633369868303021 ) ) ;
#7697 = CARTESIAN_POINT ( 'NONE',  ( -0.01814118441321365544, -2.249340926099361315, 3.500000000000000000 ) ) ;
#7698 = CARTESIAN_POINT ( 'NONE',  ( -1.467888652719046449, -0.5493409260993611376, 3.492485675378536047 ) ) ;
#7699 = ORIENTED_EDGE ( 'NONE', *, *, #4628, .T. ) ;
#7700 = CARTESIAN_POINT ( 'NONE',  ( 3.061616997868382648E-16, 76.00000000000000000, 2.499999999999999556 ) ) ;
#7701 = CARTESIAN_POINT ( 'NONE',  ( 5.114683531250000748, -29.35937500034139802, 0.000000000000000000 ) ) ;
#7702 =( BOUNDED_CURVE ( )  B_SPLINE_CURVE ( 2, ( #7608, #3891, #8810, #1795, #4029, #3194, #3285, #2592, #6665 ),
 .UNSPECIFIED., .F., .F. ) 
 B_SPLINE_CURVE_WITH_KNOTS ( ( 3, 2, 2, 2, 3 ),
 ( 0.2708333333333333703, 0.2777777777777777901, 0.2916666666666666852, 0.3055555555555555802, 0.3125000000000000000 ),
 .UNSPECIFIED. ) 
 CURVE ( )  GEOMETRIC_REPRESENTATION_ITEM ( )  RATIONAL_B_SPLINE_CURVE ( ( 0.9330127018922194093, 0.9330127018922196314, 1.000000000000000000, 0.8660254037844387076, 1.000000000000000000, 0.8660254037844387076, 1.000000000000000000, 0.9330127018922194093, 0.9330127018922194093 ) ) 
 REPRESENTATION_ITEM ( '' )  );
#7703 = CARTESIAN_POINT ( 'NONE',  ( 5.385316468750000141, -29.98437499965859843, -6.595110575850215044E-16 ) ) ;
#7704 = ADVANCED_FACE ( 'NONE', ( #6127 ), #2696, .F. ) ;
#7705 = VERTEX_POINT ( 'NONE', #1109 ) ;
#7706 = CARTESIAN_POINT ( 'NONE',  ( 2.692658234374998738, -29.41145833299193413, -4.663820869356206877 ) ) ;
#7707 = CARTESIAN_POINT ( 'NONE',  ( 1.674995433905515085, -1.850659073900638774, 3.992485675378568022 ) ) ;
#7708 = LINE ( 'NONE', #26, #9049 ) ;
#7709 = VECTOR ( 'NONE', #8969, 1000.000000000000000 ) ;
#7710 = CARTESIAN_POINT ( 'NONE',  ( 0.000000000000000000, -20.00000000000000000, 0.000000000000000000 ) ) ;
#7711 = DIRECTION ( 'NONE',  ( 0.000000000000000000, -1.000000000000000000, 0.000000000000000000 ) ) ;
#7712 = ADVANCED_FACE ( 'NONE', ( #8958 ), #5523, .T. ) ;
#7713 = DIRECTION ( 'NONE',  ( -0.000000000000000000, -1.000000000000000000, -0.000000000000000000 ) ) ;
#7714 = AXIS2_PLACEMENT_3D ( 'NONE', #5097, #221, #263 ) ;
#7715 = CARTESIAN_POINT ( 'NONE',  ( 2.557341765625000818, -28.31770833367473017, -4.429445870380400052 ) ) ;
#7716 = CARTESIAN_POINT ( 'NONE',  ( -5.385316468750000141, -30.10937499965859843, 0.000000000000000000 ) ) ;
#7717 = EDGE_CURVE ( 'NONE', #6430, #5221, #3996, .T. ) ;
#7718 = CARTESIAN_POINT ( 'NONE',  ( -0.01814118441320841310, -3.849340926099361404, 3.000000000000000444 ) ) ;
#7719 = CARTESIAN_POINT ( 'NONE',  ( 6.972266317189433020E-16, -29.43750000000000000, -5.249999999999999112 ) ) ;
#7720 = CARTESIAN_POINT ( 'NONE',  ( -3.807688866302469071E-16, -29.14062499965860553, -6.218427825808274356 ) ) ;
#7721 = CARTESIAN_POINT ( 'NONE',  ( -4.007514324621431534, -1.250659073900638685, -1.638713065079248521 ) ) ;
#7722 = CARTESIAN_POINT ( 'NONE',  ( 5.250000000000000888, -30.08333333265053611, 3.031088913245533423 ) ) ;
#7723 = CIRCLE ( 'NONE', #591, 4.000000000000000000 ) ;
#7724 = CARTESIAN_POINT ( 'NONE',  ( 5.250000000000000000, -27.25000000000000000, 0.000000000000000000 ) ) ;
#7725 = CARTESIAN_POINT ( 'NONE',  ( -2.625000000000002220, -27.86458333401612819, 4.546633369868302132 ) ) ;
#7726 = COLOUR_RGB ( '',0.8941176470588234615, 0.8941176470588234615, 0.8941176470588234615 ) ;
#7727 = EDGE_LOOP ( 'NONE', ( #8666, #6603, #5918, #2922, #3537, #4625, #1421, #960 ) ) ;
#7728 = FILL_AREA_STYLE ('',( #8473 ) ) ;
#7729 =( GEOMETRIC_REPRESENTATION_CONTEXT ( 3 ) GLOBAL_UNCERTAINTY_ASSIGNED_CONTEXT ( ( #5891 ) ) GLOBAL_UNIT_ASSIGNED_CONTEXT ( ( #6946, #3420, #7556 ) ) REPRESENTATION_CONTEXT ( 'NONE', 'WORKASPACE' ) );
#7730 = CARTESIAN_POINT ( 'NONE',  ( -3.712013335537174572E-16, -29.56250000000000000, -6.062177826491070398 ) ) ;
#7731 = ORIENTED_EDGE ( 'NONE', *, *, #4101, .F. ) ;
#7732 = CARTESIAN_POINT ( 'NONE',  ( -2.557341765624999042, -28.27604166700806587, -4.429445870380400052 ) ) ;
#7733 = CARTESIAN_POINT ( 'NONE',  ( -3.007514324621435531, -2.850659073900640106, -1.224499502706142273 ) ) ;
#7734 = AXIS2_PLACEMENT_3D ( 'NONE', #5075, #805, #2251 ) ;
#7735 = CARTESIAN_POINT ( 'NONE',  ( 5.114683531250000748, -26.92187500034139802, 0.000000000000000000 ) ) ;
#7736 = DIRECTION ( 'NONE',  ( 0.000000000000000000, -0.000000000000000000, -1.000000000000000000 ) ) ;
#7737 = CARTESIAN_POINT ( 'NONE',  ( 2.557341765624996821, -28.96354166700806587, 4.429445870380401828 ) ) ;
#7738 = VECTOR ( 'NONE', #3314, 1000.000000000000000 ) ;
#7739 = CARTESIAN_POINT ( 'NONE',  ( 6.429395695523604153E-16, -27.00000000000000000, 5.250000000000000000 ) ) ;
#7740 = CARTESIAN_POINT ( 'NONE',  ( -5.114683531250000748, -27.27604166700806232, 2.952963913586931888 ) ) ;
#7741 = CARTESIAN_POINT ( 'NONE',  ( -5.249999999999999112, -29.64583333333333215, -3.031088913245536975 ) ) ;
#7742 = EDGE_CURVE ( 'NONE', #6258, #7207, #2661, .T. ) ;
#7743 = CARTESIAN_POINT ( 'NONE',  ( 5.250000000000000888, -29.58333333265053611, 3.031088913245532979 ) ) ;
#7744 = CARTESIAN_POINT ( 'NONE',  ( 0.000000000000000000, 74.00000000000001421, 0.000000000000000000 ) ) ;
#7745 = CARTESIAN_POINT ( 'NONE',  ( 3.500000000000000000, -2.649340926099361226, 0.01814118441321387054 ) ) ;
#7746 = CARTESIAN_POINT ( 'NONE',  ( 3.492485675378536047, -4.149340926099361226, 1.467888652719046672 ) ) ;
#7747 = ORIENTED_EDGE ( 'NONE', *, *, #1863, .F. ) ;
#7748 = AXIS2_PLACEMENT_3D ( 'NONE', #2788, #7054, #8502 ) ;
#7749 = CARTESIAN_POINT ( 'NONE',  ( -5.249999999999997335, -29.66666666598386826, 3.031088913245538308 ) ) ;
#7750 = PRODUCT_RELATED_PRODUCT_CATEGORY ( 'part', '', ( #4156 ) ) ;
#7751 = CARTESIAN_POINT ( 'NONE',  ( 3.616337804771879580E-16, -29.79687500034140157, -5.905927827173866440 ) ) ;
#7752 = ORIENTED_EDGE ( 'NONE', *, *, #2549, .F. ) ;
#7753 = CARTESIAN_POINT ( 'NONE',  ( -5.385316468749998364, -29.80729166632526628, 3.109213912904140287 ) ) ;
#7754 = CARTESIAN_POINT ( 'NONE',  ( -2.815599370228907272, -1.550659073900638507, 2.841254879263473754 ) ) ;
#7755 = DIRECTION ( 'NONE',  ( -0.000000000000000000, 1.000000000000000000, -0.000000000000000000 ) ) ;
#7756 = ORIENTED_EDGE ( 'NONE', *, *, #3267, .F. ) ;
#7757 = DIRECTION ( 'NONE',  ( 0.000000000000000000, 0.000000000000000000, -1.000000000000000000 ) ) ;
#7758 = CARTESIAN_POINT ( 'NONE',  ( -3.500000000000000000, -8.249340926099360871, -0.01814118441321344033 ) ) ;
#7759 = ADVANCED_FACE ( 'NONE', ( #6924 ), #3251, .T. ) ;
#7760 = CARTESIAN_POINT ( 'NONE',  ( 3.616337804771879580E-16, -28.79687500034139802, -5.905927827173866440 ) ) ;
#7761 = DIRECTION ( 'NONE',  ( -0.000000000000000000, -1.000000000000000000, -0.000000000000000000 ) ) ;
#7762 = CARTESIAN_POINT ( 'NONE',  ( -5.250000000000000000, -28.68749999931720396, 0.000000000000000000 ) ) ;
#7763 = CARTESIAN_POINT ( 'NONE',  ( 3.000000000000000444, -7.449340926099361937, 0.01814118441320859698 ) ) ;
#7764 = EDGE_CURVE ( 'NONE', #5384, #1844, #7115, .T. ) ;
#7765 = CARTESIAN_POINT ( 'NONE',  ( 0.000000000000000000, -35.00000000000000000, 0.000000000000000000 ) ) ;
#7766 = CARTESIAN_POINT ( 'NONE',  ( -3.807688866302469071E-16, -27.17187499965860198, -6.218427825808274356 ) ) ;
#7767 = CARTESIAN_POINT ( 'NONE',  ( -2.815599370228907272, 0.04934092609936149149, 2.841254879263473754 ) ) ;
#7768 = AXIS2_PLACEMENT_3D ( 'NONE', #8440, #4118, #624 ) ;
#7769 = DIRECTION ( 'NONE',  ( 0.000000000000000000, -0.000000000000000000, 1.000000000000000000 ) ) ;
#7770 = EDGE_CURVE ( 'NONE', #7184, #6870, #3119, .T. ) ;
#7771 = DIRECTION ( 'NONE',  ( 0.000000000000000000, 0.000000000000000000, 1.000000000000000000 ) ) ;
#7772 = ORIENTED_EDGE ( 'NONE', *, *, #2843, .T. ) ;
#7773 = AXIS2_PLACEMENT_3D ( 'NONE', #4643, #2560, #7484 ) ;
#7774 =( LENGTH_UNIT ( ) NAMED_UNIT ( * ) SI_UNIT ( .MILLI., .METRE. ) );
#7775 = CARTESIAN_POINT ( 'NONE',  ( -2.625000000000000444, -29.54166666666666785, -4.546633369868303021 ) ) ;
#7776 = AXIS2_PLACEMENT_3D ( 'NONE', #8438, #2064, #4249 ) ;
#7777 = CARTESIAN_POINT ( 'NONE',  ( 5.114683531250000748, -28.10937500034139447, 0.000000000000000000 ) ) ;
#7778 = CARTESIAN_POINT ( 'NONE',  ( 1.224499502706142273, -0.8506590739006396618, -3.007514324621435531 ) ) ;
#7779 = CARTESIAN_POINT ( 'NONE',  ( 5.249999999999999112, -29.77083333333333570, 3.031088913245538308 ) ) ;
#7780 = DIRECTION ( 'NONE',  ( -0.000000000000000000, 1.000000000000000000, -0.000000000000000000 ) ) ;
#7781 = ADVANCED_FACE ( 'NONE', ( #2609 ), #2558, .F. ) ;
#7782 =( BOUNDED_SURFACE ( )  B_SPLINE_SURFACE ( 1, 2, ( 
 ( #5760, #7116, #6604, #2233, #4467, #7957, #233, #6554, #184, #5108, #5812, #5058, #49, #3633, #5904, #8743, #5858, #6455, #7911, #7821, #4376, #3586, #6410, #7208, #5715, #5008, #137, #3678, #6500, #2988, #8650, #4651, #1725, #8146, #1676, #6691, #1020, #3915, #5295, #1072, #3821, #5206, #3870, #6739, #370, #321, #6787, #8835, #7447, #4609, #3173, #7349, #1163, #7397, #5996, #1773, #3129, #5342, #2471, #8048, #4562, #275, #3218, #7494, #413, #6038, #4007, #8791, #1119, #2377, #8875, #6841, #2516, #3261, #3961, #8191, #1820, #6089, #2422, #3310, #8922, #2571, #5389, #8240, #4697, #4520, #5252, #1874, #975, #8097, #7537, #465, #5952, #6141, #6646, #4741, #2093, #3405, #8420, #7720, #2047, #4832, #8970, #3359, #9066, #4232, #7063, #4054, #9110, #2755, #3490, #604, #8332, #6234, #7588, #8282, #1214, #4918, #516, #3448, #6274, #6189, #687, #6933, #9017, #3533, #1348, #2663, #1389, #2706, #2620, #7019, #6889, #4873, #6975, #2799, #5485, #5576, #644, #4186, #5535, #6315, #1917, #5437, #8378 ),
 ( #9151, #1963, #4789, #7766, #7633, #5617, #2007, #8465, #1261, #4100, #561, #7678, #1300, #4142, #2400, #6447, #4274, #5706, #2845, #3154, #5972, #2451, #7107, #8769, #4999, #5277, #778, #4366, #8121, #8074, #39, #5929, #3104, #4319, #5664, #1751, #3625, #300, #253, #998, #5229, #1703, #6492, #7200, #7155, #1430, #8550, #4586, #8814, #4541, #2889, #81, #7373, #2178, #7424, #8510, #8593, #2931, #3578, #1047, #3844, #730, #6357, #5752, #4868, #6669, #6403, #2136, #824, #4958, #7855, #3667, #7813, #1476, #2222, #5048, #7903, #1522, #7515, #347, #491, #1189, #6914, #6117, #8993, #7612, #8308, #4678, #2495, #8946, #538, #6714, #2598, #4078, #4768, #6019, #1144, #3379, #6167, #7657, #3198, #2641, #5415, #8264, #2545, #1895, #7563, #6212, #1236, #9041, #4632, #8856, #442, #4722, #7470, #1099, #3987, #3289, #2683, #1798, #8899, #3895, #6816, #6065, #5317, #4033, #8170, #5513, #394, #8356, #3939, #5462, #6766, #1981, #4812, #3241, #5368, #8217, #1939, #1851, #6867, #3338, #706, #1411, #6334 ) ),
 .UNSPECIFIED., .F., .F., .T. ) 
 B_SPLINE_SURFACE_WITH_KNOTS ( ( 2, 2 ),
 ( 3, 2, 2, 2, 2, 2, 2, 2, 2, 2, 2, 2, 2, 2, 2, 2, 2, 2, 2, 2, 2, 2, 2, 2, 2, 2, 2, 2, 2, 2, 2, 2, 2, 2, 2, 2, 2, 2, 2, 2, 2, 2, 2, 2, 2, 2, 2, 2, 2, 2, 2, 2, 2, 2, 2, 2, 2, 2, 2, 2, 2, 2, 2, 2, 2, 2, 2, 2, 2, 2, 2, 2, 3 ),
 ( 0.000000000000000000, 1.000000000000000000 ),
 ( 0.000000000000000000, 0.01388888888888888812, 0.02777777777777777624, 0.04166666666666666435, 0.05555555555555555247, 0.06944444444444444753, 0.08333333333333332871, 0.09722222222222222376, 0.1111111111111111049, 0.1250000000000000000, 0.1388888888888888951, 0.1527777777777777901, 0.1666666666666666574, 0.1805555555555555525, 0.1944444444444444475, 0.2083333333333333426, 0.2222222222222222099, 0.2361111111111111049, 0.2500000000000000000, 0.2638888888888888951, 0.2777777777777777901, 0.2916666666666666852, 0.3055555555555555802, 0.3194444444444444198, 0.3333333333333333148, 0.3472222222222222099, 0.3611111111111111049, 0.3750000000000000000, 0.3888888888888888951, 0.4027777777777777901, 0.4166666666666666852, 0.4305555555555555802, 0.4444444444444444198, 0.4583333333333333148, 0.4722222222222222099, 0.4861111111111111049, 0.5000000000000000000, 0.5138888888888888395, 0.5277777777777777901, 0.5416666666666666297, 0.5555555555555555802, 0.5694444444444444198, 0.5833333333333333703, 0.5972222222222222099, 0.6111111111111111605, 0.6250000000000000000, 0.6388888888888888395, 0.6527777777777777901, 0.6666666666666666297, 0.6805555555555555802, 0.6944444444444444198, 0.7083333333333333703, 0.7222222222222222099, 0.7361111111111111605, 0.7500000000000000000, 0.7638888888888888395, 0.7777777777777777901, 0.7916666666666666297, 0.8055555555555555802, 0.8194444444444444198, 0.8333333333333333703, 0.8472222222222222099, 0.8611111111111111605, 0.8750000000000000000, 0.8888888888888888395, 0.9027777777777777901, 0.9166666666666666297, 0.9305555555555555802, 0.9444444444444444198, 0.9583333333333333703, 0.9722222222222222099, 0.9861111111111111605, 1.000000000000000000 ),
 .UNSPECIFIED. ) 
 GEOMETRIC_REPRESENTATION_ITEM ( )  RATIONAL_B_SPLINE_SURFACE ( (
 ( 1.000000000000000000, 0.8660254037844387076, 1.000000000000000000, 0.8660254037844387076, 1.000000000000000000, 0.8660254037844387076, 1.000000000000000000, 0.8660254037844387076, 1.000000000000000000, 0.8660254037844387076, 1.000000000000000000, 0.8660254037844387076, 1.000000000000000000, 0.8660254037844387076, 1.000000000000000000, 0.8660254037844387076, 1.000000000000000000, 0.8660254037844387076, 1.000000000000000000, 0.8660254037844387076, 1.000000000000000000, 0.8660254037844387076, 1.000000000000000000, 0.8660254037844387076, 1.000000000000000000, 0.8660254037844387076, 1.000000000000000000, 0.8660254037844387076, 1.000000000000000000, 0.8660254037844387076, 1.000000000000000000, 0.8660254037844387076, 1.000000000000000000, 0.8660254037844387076, 1.000000000000000000, 0.8660254037844387076, 1.000000000000000000, 0.8660254037844387076, 1.000000000000000000, 0.8660254037844387076, 1.000000000000000000, 0.8660254037844387076, 1.000000000000000000, 0.8660254037844387076, 1.000000000000000000, 0.8660254037844387076, 1.000000000000000000, 0.8660254037844387076, 1.000000000000000000, 0.8660254037844387076, 1.000000000000000000, 0.8660254037844387076, 1.000000000000000000, 0.8660254037844387076, 1.000000000000000000, 0.8660254037844387076, 1.000000000000000000, 0.8660254037844387076, 1.000000000000000000, 0.8660254037844387076, 1.000000000000000000, 0.8660254037844387076, 1.000000000000000000, 0.8660254037844387076, 1.000000000000000000, 0.8660254037844387076, 1.000000000000000000, 0.8660254037844387076, 1.000000000000000000, 0.8660254037844387076, 1.000000000000000000, 0.8660254037844387076, 1.000000000000000000, 0.8660254037844387076, 1.000000000000000000, 0.8660254037844387076, 1.000000000000000000, 0.8660254037844387076, 1.000000000000000000, 0.8660254037844387076, 1.000000000000000000, 0.8660254037844387076, 1.000000000000000000, 0.8660254037844387076, 1.000000000000000000, 0.8660254037844387076, 1.000000000000000000, 0.8660254037844387076, 1.000000000000000000, 0.8660254037844387076, 1.000000000000000000, 0.8660254037844387076, 1.000000000000000000, 0.8660254037844387076, 1.000000000000000000, 0.8660254037844387076, 1.000000000000000000, 0.8660254037844387076, 1.000000000000000000, 0.8660254037844387076, 1.000000000000000000, 0.8660254037844387076, 1.000000000000000000, 0.8660254037844387076, 1.000000000000000000, 0.8660254037844387076, 1.000000000000000000, 0.8660254037844387076, 1.000000000000000000, 0.8660254037844387076, 1.000000000000000000, 0.8660254037844387076, 1.000000000000000000, 0.8660254037844387076, 1.000000000000000000, 0.8660254037844387076, 1.000000000000000000, 0.8660254037844387076, 1.000000000000000000, 0.8660254037844387076, 1.000000000000000000, 0.8660254037844387076, 1.000000000000000000, 0.8660254037844387076, 1.000000000000000000, 0.8660254037844387076, 1.000000000000000000, 0.8660254037844387076, 1.000000000000000000, 0.8660254037844387076, 1.000000000000000000, 0.8660254037844387076, 1.000000000000000000, 0.8660254037844387076, 1.000000000000000000, 0.8660254037844387076, 1.000000000000000000, 0.8660254037844387076, 1.000000000000000000, 0.8660254037844387076, 1.000000000000000000, 0.8660254037844387076, 1.000000000000000000, 0.8660254037844387076, 1.000000000000000000),
 ( 1.000000000000000000, 0.8660254037844387076, 1.000000000000000000, 0.8660254037844387076, 1.000000000000000000, 0.8660254037844387076, 1.000000000000000000, 0.8660254037844387076, 1.000000000000000000, 0.8660254037844387076, 1.000000000000000000, 0.8660254037844387076, 1.000000000000000000, 0.8660254037844387076, 1.000000000000000000, 0.8660254037844387076, 1.000000000000000000, 0.8660254037844387076, 1.000000000000000000, 0.8660254037844387076, 1.000000000000000000, 0.8660254037844387076, 1.000000000000000000, 0.8660254037844387076, 1.000000000000000000, 0.8660254037844387076, 1.000000000000000000, 0.8660254037844387076, 1.000000000000000000, 0.8660254037844387076, 1.000000000000000000, 0.8660254037844387076, 1.000000000000000000, 0.8660254037844387076, 1.000000000000000000, 0.8660254037844387076, 1.000000000000000000, 0.8660254037844387076, 1.000000000000000000, 0.8660254037844387076, 1.000000000000000000, 0.8660254037844387076, 1.000000000000000000, 0.8660254037844387076, 1.000000000000000000, 0.8660254037844387076, 1.000000000000000000, 0.8660254037844387076, 1.000000000000000000, 0.8660254037844387076, 1.000000000000000000, 0.8660254037844387076, 1.000000000000000000, 0.8660254037844387076, 1.000000000000000000, 0.8660254037844387076, 1.000000000000000000, 0.8660254037844387076, 1.000000000000000000, 0.8660254037844387076, 1.000000000000000000, 0.8660254037844387076, 1.000000000000000000, 0.8660254037844387076, 1.000000000000000000, 0.8660254037844387076, 1.000000000000000000, 0.8660254037844387076, 1.000000000000000000, 0.8660254037844387076, 1.000000000000000000, 0.8660254037844387076, 1.000000000000000000, 0.8660254037844387076, 1.000000000000000000, 0.8660254037844387076, 1.000000000000000000, 0.8660254037844387076, 1.000000000000000000, 0.8660254037844387076, 1.000000000000000000, 0.8660254037844387076, 1.000000000000000000, 0.8660254037844387076, 1.000000000000000000, 0.8660254037844387076, 1.000000000000000000, 0.8660254037844387076, 1.000000000000000000, 0.8660254037844387076, 1.000000000000000000, 0.8660254037844387076, 1.000000000000000000, 0.8660254037844387076, 1.000000000000000000, 0.8660254037844387076, 1.000000000000000000, 0.8660254037844387076, 1.000000000000000000, 0.8660254037844387076, 1.000000000000000000, 0.8660254037844387076, 1.000000000000000000, 0.8660254037844387076, 1.000000000000000000, 0.8660254037844387076, 1.000000000000000000, 0.8660254037844387076, 1.000000000000000000, 0.8660254037844387076, 1.000000000000000000, 0.8660254037844387076, 1.000000000000000000, 0.8660254037844387076, 1.000000000000000000, 0.8660254037844387076, 1.000000000000000000, 0.8660254037844387076, 1.000000000000000000, 0.8660254037844387076, 1.000000000000000000, 0.8660254037844387076, 1.000000000000000000, 0.8660254037844387076, 1.000000000000000000, 0.8660254037844387076, 1.000000000000000000, 0.8660254037844387076, 1.000000000000000000, 0.8660254037844387076, 1.000000000000000000, 0.8660254037844387076, 1.000000000000000000, 0.8660254037844387076, 1.000000000000000000, 0.8660254037844387076, 1.000000000000000000, 0.8660254037844387076, 1.000000000000000000, 0.8660254037844387076, 1.000000000000000000, 0.8660254037844387076, 1.000000000000000000, 0.8660254037844387076, 1.000000000000000000) ) ) 
 REPRESENTATION_ITEM ( '' )  SURFACE ( )  );
#7783 = AXIS2_PLACEMENT_3D ( 'NONE', #24, #1993, #903 ) ;
#7784 = CARTESIAN_POINT ( 'NONE',  ( -5.114683531250001636, -29.27604166700806232, 2.952963913586931444 ) ) ;
#7785 = EDGE_CURVE ( 'NONE', #3890, #6474, #1182, .T. ) ;
#7786 = SHAPE_REPRESENTATION_RELATIONSHIP ( 'NONE' , 'NONE' ,  #1697, #542 ) ;
#7787 = CARTESIAN_POINT ( 'NONE',  ( 2.557341765625000818, -27.13020833367473017, -4.429445870380400052 ) ) ;
#7788 = DIRECTION ( 'NONE',  ( 0.000000000000000000, -1.000000000000000000, 0.000000000000000000 ) ) ;
#7789 = EDGE_CURVE ( 'NONE', #2627, #8711, #5378, .T. ) ;
#7790 = CARTESIAN_POINT ( 'NONE',  ( 2.625000000000002220, -29.10416666598386826, 4.546633369868302132 ) ) ;
#7791 = DIRECTION ( 'NONE',  ( 0.000000000000000000, -1.000000000000000000, 0.000000000000000000 ) ) ;
#7792 = AXIS2_PLACEMENT_3D ( 'NONE', #7419, #438, #4627 ) ;
#7793 = CARTESIAN_POINT ( 'NONE',  ( 2.161402558328724325E-14, -28.81250000000000000, -5.250000000000000000 ) ) ;
#7794 = DIRECTION ( 'NONE',  ( 0.000000000000000000, 0.000000000000000000, 1.000000000000000000 ) ) ;
#7795 = CARTESIAN_POINT ( 'NONE',  ( 2.462045979635577364, -7.249340926099360871, 2.487701488670255312 ) ) ;
#7796 = CARTESIAN_POINT ( 'NONE',  ( -1.431606283892620235, -6.349340926099360516, -3.507514324621463953 ) ) ;
#7797 = ORIENTED_EDGE ( 'NONE', *, *, #8371, .F. ) ;
#7798 = PLANE ( 'NONE',  #8019 ) ;
#7799 = CARTESIAN_POINT ( 'NONE',  ( -5.250000000000000000, -27.15625000068279604, -6.429395695523604153E-16 ) ) ;
#7800 = VERTEX_POINT ( 'NONE', #1810 ) ;
#7801 = CARTESIAN_POINT ( 'NONE',  ( 5.385316468749999252, -29.93229166632526983, -3.109213912904138954 ) ) ;
#7802 = CARTESIAN_POINT ( 'NONE',  ( 4.007514324621432422, -2.050659073900638507, 1.638713065079246078 ) ) ;
#7803 = DIRECTION ( 'NONE',  ( 0.000000000000000000, -0.000000000000000000, 1.000000000000000000 ) ) ;
#7804 = ORIENTED_EDGE ( 'NONE', *, *, #8959, .F. ) ;
#7805 = CARTESIAN_POINT ( 'NONE',  ( -2.033577675846918216E-14, -29.12499999931720751, 5.250000000000000888 ) ) ;
#7806 = PLANE ( 'NONE',  #2393 ) ;
#7807 = CARTESIAN_POINT ( 'NONE',  ( 1.406733260263395735, -27.36383544963256753, 5.250000000000000000 ) ) ;
#7808 = CARTESIAN_POINT ( 'NONE',  ( 2.557341765625000818, -28.56770833367473017, -4.429445870380400052 ) ) ;
#7809 = FACE_OUTER_BOUND ( 'NONE', #1858, .T. ) ;
#7810 = CARTESIAN_POINT ( 'NONE',  ( 1.406733260263391960, -29.08258545099816317, 5.250000000000000000 ) ) ;
#7811 = CARTESIAN_POINT ( 'NONE',  ( 2.992485675378538712, -2.549340926099361582, 1.260781871532494103 ) ) ;
#7812 = CARTESIAN_POINT ( 'NONE',  ( 1.406733260263395735, -28.67633545031537068, 5.250000000000000000 ) ) ;
#7813 = CARTESIAN_POINT ( 'NONE',  ( -5.385316468750000141, -28.60937499965860198, 0.000000000000000000 ) ) ;
#7814 = CARTESIAN_POINT ( 'NONE',  ( -3.992485675378568022, 0.1493409260993615040, 1.674995433905515529 ) ) ;
#7815 = CARTESIAN_POINT ( 'NONE',  ( 6.972266317189433020E-16, -27.18750000000000000, -5.250000000000000000 ) ) ;
#7816 = LINE ( 'NONE', #2934, #8912 ) ;
#7817 = EDGE_CURVE ( 'NONE', #4147, #1378, #5767, .T. ) ;
#7818 = EDGE_LOOP ( 'NONE', ( #6347, #2496, #5648, #1947 ) ) ;
#7819 = CARTESIAN_POINT ( 'NONE',  ( -5.385316468749998364, -27.30729166632526983, 3.109213912904140287 ) ) ;
#7820 = VERTEX_POINT ( 'NONE', #3300 ) ;
#7821 = CARTESIAN_POINT ( 'NONE',  ( 5.385316468750001029, -27.47395833299193413, 3.109213912904135846 ) ) ;
#7822 = CARTESIAN_POINT ( 'NONE',  ( 3.000000000000000444, -7.449340926099361937, 0.01814118441320859698 ) ) ;
#7823 = ORIENTED_EDGE ( 'NONE', *, *, #4776, .F. ) ;
#7824 = CARTESIAN_POINT ( 'NONE',  ( 5.250000000000000000, -28.99999999999999645, 0.000000000000000000 ) ) ;
#7825 = CARTESIAN_POINT ( 'NONE',  ( 3.122849337825750419E-16, -53.00000000000000000, -2.549999999999999822 ) ) ;
#7826 = CARTESIAN_POINT ( 'NONE',  ( -5.114683531250000748, -29.54687500034139802, -6.263680815196995234E-16 ) ) ;
#7827 = CARTESIAN_POINT ( 'NONE',  ( -2.557341765625002594, -28.00520833367473017, 4.429445870380399164 ) ) ;
#7828 = CARTESIAN_POINT ( 'NONE',  ( -2.624999999999996891, -29.89583333265053611, 4.546633369868304797 ) ) ;
#7829 = PRODUCT ( 'MAS-161', 'MAS-161', '', ( #6837 ) ) ;
#7830 = FACE_OUTER_BOUND ( 'NONE', #8721, .T. ) ;
#7831 = CARTESIAN_POINT ( 'NONE',  ( -3.551368067147179008, -3.053917841153461118E-13, 1.202414619655959971 ) ) ;
#7832 = CARTESIAN_POINT ( 'NONE',  ( 1.406733260263397289, -28.55133545031537068, 5.249999999999997335 ) ) ;
#7833 = CARTESIAN_POINT ( 'NONE',  ( -5.249999999999999112, -29.67708333401613530, -3.031088913245536975 ) ) ;
#7834 =( BOUNDED_CURVE ( )  B_SPLINE_CURVE ( 2, ( #3222, #8016, #1502, #1647, #4345, #1076, #7181, #3648, #6278 ),
 .UNSPECIFIED., .F., .T. ) 
 B_SPLINE_CURVE_WITH_KNOTS ( ( 3, 2, 2, 2, 3 ),
 ( 0.3541666666666666297, 0.3611111111111111049, 0.3750000000000000000, 0.3888888888888888951, 0.3958333333333333703 ),
 .UNSPECIFIED. ) 
 CURVE ( )  GEOMETRIC_REPRESENTATION_ITEM ( )  RATIONAL_B_SPLINE_CURVE ( ( 0.9330127018922194093, 0.9330127018922190762, 1.000000000000000000, 0.8660254037844387076, 1.000000000000000000, 0.8660254037844387076, 1.000000000000000000, 0.9330127018922190762, 0.9330127018922194093 ) ) 
 REPRESENTATION_ITEM ( '' )  );
#7835 = CARTESIAN_POINT ( 'NONE',  ( 1.467888652719048226, -6.149340926099360338, -3.492485675378536047 ) ) ;
#7836 = ORIENTED_EDGE ( 'NONE', *, *, #2778, .F. ) ;
#7837 = FACE_OUTER_BOUND ( 'NONE', #8770, .T. ) ;
#7838 = CARTESIAN_POINT ( 'NONE',  ( -1.084901341431563923E-15, -29.42187500034139447, 5.905927827173866440 ) ) ;
#7839 = ORIENTED_EDGE ( 'NONE', *, *, #7269, .T. ) ;
#7840 = COLOUR_RGB ( '',0.8941176470588234615, 0.8941176470588234615, 0.8941176470588234615 ) ;
#7841 = ORIENTED_EDGE ( 'NONE', *, *, #8041, .T. ) ;
#7842 = CARTESIAN_POINT ( 'NONE',  ( -5.385316468750000141, -29.57812499965859843, 0.000000000000000000 ) ) ;
#7843 = CARTESIAN_POINT ( 'NONE',  ( 3.500000000000000000, -6.950659073900639306, -0.01814118441313969030 ) ) ;
#7844 = CARTESIAN_POINT ( 'NONE',  ( 1.975475456537005874E-15, -28.87499999931720396, 5.249999999999999112 ) ) ;
#7845 = ORIENTED_EDGE ( 'NONE', *, *, #6337, .T. ) ;
#7846 = COLOUR_RGB ( '',0.8941176470588234615, 0.8941176470588234615, 0.8941176470588234615 ) ;
#7847 = CARTESIAN_POINT ( 'NONE',  ( 2.300847884672513123E-14, -27.96875000068279959, -5.250000000000000000 ) ) ;
#7848 = DIRECTION ( 'NONE',  ( 0.000000000000000000, -1.000000000000000000, 0.000000000000000000 ) ) ;
#7849 = CYLINDRICAL_SURFACE ( 'NONE', #7435, 2.499999999999999556 ) ;
#7850 = CARTESIAN_POINT ( 'NONE',  ( 5.114683531250000748, -28.10937500034139447, 0.000000000000000000 ) ) ;
#7851 = CARTESIAN_POINT ( 'NONE',  ( 2.487701488670255756, -2.849340926099361404, -2.462045979635577364 ) ) ;
#7852 = DIRECTION ( 'NONE',  ( 0.000000000000000000, 1.000000000000000000, 0.000000000000000000 ) ) ;
#7853 = CARTESIAN_POINT ( 'NONE',  ( 2.992485675378538712, -4.149340926099362115, 1.260781871532494103 ) ) ;
#7854 = CARTESIAN_POINT ( 'NONE',  ( 5.250000000000000000, -28.62500000000000000, -6.429395695523604153E-16 ) ) ;
#7855 = CARTESIAN_POINT ( 'NONE',  ( -2.692658234374996518, -28.56770833299193413, 4.663820869356208654 ) ) ;
#7856 = EDGE_CURVE ( 'NONE', #3802, #2565, #3904, .T. ) ;
#7857 = CARTESIAN_POINT ( 'NONE',  ( 3.992485675378533383, -2.549340926099360694, 1.674995433905599462 ) ) ;
#7858 = AXIS2_PLACEMENT_3D ( 'NONE', #2022, #7080, #3422 ) ;
#7859 = CARTESIAN_POINT ( 'NONE',  ( -5.250000000000000000, -27.65625000068279959, -6.429395695523604153E-16 ) ) ;
#7860 = VERTEX_POINT ( 'NONE', #8321 ) ;
#7861 =( NAMED_UNIT ( * ) PLANE_ANGLE_UNIT ( ) SI_UNIT ( $, .RADIAN. ) );
#7862 = CARTESIAN_POINT ( 'NONE',  ( 2.625000000000002220, -29.91666666666666785, 4.546633369868302132 ) ) ;
#7863 = VERTEX_POINT ( 'NONE', #1950 ) ;
#7864 = CARTESIAN_POINT ( 'NONE',  ( -1.406733260263391960, -27.19866454968463287, 5.250000000000000000 ) ) ;
#7865 = CARTESIAN_POINT ( 'NONE',  ( 2.992485675378565357, -2.250659073900640461, -1.260781871532430376 ) ) ;
#7866 = VERTEX_POINT ( 'NONE', #4780 ) ;
#7867 = CARTESIAN_POINT ( 'NONE',  ( -1.113604000661152470E-15, -29.31249999999999645, 6.062177826491070398 ) ) ;
#7868 = CARTESIAN_POINT ( 'NONE',  ( 5.250000000000000000, -29.37500000000000000, -6.429395695523604153E-16 ) ) ;
#7869 = CARTESIAN_POINT ( 'NONE',  ( -5.114683531250000748, -28.29687500034139447, -6.263680815196995234E-16 ) ) ;
#7870 = AXIS2_PLACEMENT_3D ( 'NONE', #8889, #6051, #3186 ) ;
#7871 = CLOSED_SHELL ( 'NONE', ( #9140, #1043, #8, #7560, #6989, #8288, #5068, #8606, #4588, #7712, #1761, #5595, #7367, #1567, #1838, #4068, #6385, #4688, #7033, #6959, #2593, #4072, #5331, #2712, #6406, #6107, #3591, #6128, #826, #7759, #4637, #5496, #4942, #2140, #5135, #419, #7234, #2048, #2182, #4161, #8101, #1953, #4237, #1110, #553, #5800, #1468 ) ) ;
#7872 =( NAMED_UNIT ( * ) PLANE_ANGLE_UNIT ( ) SI_UNIT ( $, .RADIAN. ) );
#7873 = CARTESIAN_POINT ( 'NONE',  ( 2.557341765624996821, -27.46354166700806587, 4.429445870380401828 ) ) ;
#7874 = CIRCLE ( 'NONE', #8026, 5.250000000000000000 ) ;
#7875 = CARTESIAN_POINT ( 'NONE',  ( -1.000000000000000000, -29.00000000000000355, 2.431755684948965435 ) ) ;
#7876 = CARTESIAN_POINT ( 'NONE',  ( 0.000000000000000000, -9.999999999999998224, 0.000000000000000000 ) ) ;
#7877 = DIRECTION ( 'NONE',  ( 0.000000000000000000, -1.000000000000000000, 0.000000000000000000 ) ) ;
#7878 = CARTESIAN_POINT ( 'NONE',  ( 1.045839947578414884E-14, -27.81249999999999289, -5.250000000000000000 ) ) ;
#7879 = CARTESIAN_POINT ( 'NONE',  ( 3.500000000000000000, -7.449340926099361937, 0.01814118441321387054 ) ) ;
#7880 = CARTESIAN_POINT ( 'NONE',  ( 2.487701488670255756, -6.049340926099361582, -2.462045979635577364 ) ) ;
#7881 = ORIENTED_EDGE ( 'NONE', *, *, #872, .F. ) ;
#7882 = FACE_OUTER_BOUND ( 'NONE', #2183, .T. ) ;
#7883 = DIRECTION ( 'NONE',  ( -0.000000000000000000, -1.000000000000000000, -0.000000000000000000 ) ) ;
#7884 = AXIS2_PLACEMENT_3D ( 'NONE', #3628, #7157, #6494 ) ;
#7885 = CARTESIAN_POINT ( 'NONE',  ( 2.557341765624996821, -27.90104166700806587, 4.429445870380401828 ) ) ;
#7886 = EDGE_CURVE ( 'NONE', #8948, #4503, #6364, .T. ) ;
#7887 = ORIENTED_EDGE ( 'NONE', *, *, #7197, .T. ) ;
#7888 = VERTEX_POINT ( 'NONE', #4823 ) ;
#7889 = DIRECTION ( 'NONE',  ( 0.000000000000000000, 1.000000000000000000, 0.000000000000000000 ) ) ;
#7890 = CARTESIAN_POINT ( 'NONE',  ( -3.807688866302469071E-16, -27.92187499965860198, -6.218427825808274356 ) ) ;
#7891 = CARTESIAN_POINT ( 'NONE',  ( 2.815599370228907716, -0.7506590739006385737, -2.841254879263473310 ) ) ;
#7892 = CYLINDRICAL_SURFACE ( 'NONE', #2216, 2.999999999999999556 ) ;
#7893 = VECTOR ( 'NONE', #1336, 1000.000000000000000 ) ;
#7894 = ORIENTED_EDGE ( 'NONE', *, *, #2128, .T. ) ;
#7895 = CARTESIAN_POINT ( 'NONE',  ( 3.061616997868383141E-16, 74.00000000000001421, -2.500000000000000000 ) ) ;
#7896 = DIRECTION ( 'NONE',  ( 0.000000000000000000, -1.000000000000000000, 0.000000000000000000 ) ) ;
#7897 = CARTESIAN_POINT ( 'NONE',  ( -2.692658234375000514, -27.15104166632526628, -4.663820869356205989 ) ) ;
#7898 = CARTESIAN_POINT ( 'NONE',  ( 5.114683531249999859, -27.08854166700806232, -2.952963913586932776 ) ) ;
#7899 = CARTESIAN_POINT ( 'NONE',  ( -2.487701488670255312, -0.4493409260993610488, 2.462045979635577808 ) ) ;
#7900 = CARTESIAN_POINT ( 'NONE',  ( -5.385316468750000141, -27.07812499965860198, 0.000000000000000000 ) ) ;
#7901 = CARTESIAN_POINT ( 'NONE',  ( -2.108492589042306964, -3.249340926099361759, -2.134148098076978251 ) ) ;
#7902 = CYLINDRICAL_SURFACE ( 'NONE', #424, 5.250000000000000000 ) ;
#7903 = CARTESIAN_POINT ( 'NONE',  ( 2.692658234374998738, -28.69270833299193413, -4.663820869356206877 ) ) ;
#7904 = CARTESIAN_POINT ( 'NONE',  ( 4.007514324621469726, -4.349340926099361404, -1.638713065079161257 ) ) ;
#7905 = DIRECTION ( 'NONE',  ( 0.000000000000000000, -1.000000000000000000, 0.000000000000000000 ) ) ;
#7906 = CARTESIAN_POINT ( 'NONE',  ( -2.624999999999998668, -27.91666666666666430, -4.546633369868303021 ) ) ;
#7907 = CARTESIAN_POINT ( 'NONE',  ( 1.406733260263395735, -29.61383544963256753, 5.250000000000000000 ) ) ;
#7908 = ORIENTED_EDGE ( 'NONE', *, *, #9001, .T. ) ;
#7909 = CARTESIAN_POINT ( 'NONE',  ( -5.249999999999999112, -29.97916666666666430, 3.031088913245538308 ) ) ;
#7910 = VERTEX_POINT ( 'NONE', #1511 ) ;
#7911 = CARTESIAN_POINT ( 'NONE',  ( 5.385316468750000141, -27.45312499965860198, -6.595110575850215044E-16 ) ) ;
#7912 = CARTESIAN_POINT ( 'NONE',  ( 2.134148098076933397, -3.550659073900639395, 2.108492589042352261 ) ) ;
#7913 = ORIENTED_EDGE ( 'NONE', *, *, #8447, .T. ) ;
#7914 = CARTESIAN_POINT ( 'NONE',  ( 5.250000000000000000, -29.50000000000000000, 0.000000000000000000 ) ) ;
#7915 = CARTESIAN_POINT ( 'NONE',  ( 1.975475456537005874E-15, -29.43750000000000000, 5.250000000000000000 ) ) ;
#7916 = CARTESIAN_POINT ( 'NONE',  ( -2.557341765624999042, -27.58854166700806587, -4.429445870380400052 ) ) ;
#7917 = CIRCLE ( 'NONE', #8064, 2.549999999999999822 ) ;
#7918 = CARTESIAN_POINT ( 'NONE',  ( 2.557341765625000818, -27.88020833367473017, -4.429445870380400052 ) ) ;
#7919 = CARTESIAN_POINT ( 'NONE',  ( -2.557341765625002594, -29.69270833367473017, 4.429445870380399164 ) ) ;
#7920 = CARTESIAN_POINT ( 'NONE',  ( 2.462045979635577364, -4.049340926099360694, 2.487701488670255312 ) ) ;
#7921 = LINE ( 'NONE', #1689, #8761 ) ;
#7922 = CIRCLE ( 'NONE', #4508, 1.499999999999999778 ) ;
#7923 = CARTESIAN_POINT ( 'NONE',  ( -9.180150650966086169E-15, -28.18749999999999645, 5.250000000000000000 ) ) ;
#7924 = CARTESIAN_POINT ( 'NONE',  ( 5.114683531250000748, -29.42187500034139802, 0.000000000000000000 ) ) ;
#7925 = CYLINDRICAL_SURFACE ( 'NONE', #1991, 2.750000000000000000 ) ;
#7926 = EDGE_CURVE ( 'NONE', #784, #5221, #1346, .T. ) ;
#7927 = ORIENTED_EDGE ( 'NONE', *, *, #4524, .T. ) ;
#7928 = CARTESIAN_POINT ( 'NONE',  ( 1.045839947578414884E-14, -27.99999999931720041, -5.250000000000000000 ) ) ;
#7929 = CARTESIAN_POINT ( 'NONE',  ( 0.000000000000000000, 69.99999999999998579, 0.000000000000000000 ) ) ;
#7930 = CARTESIAN_POINT ( 'NONE',  ( 5.114683531249998971, -28.38020833367473372, 2.952963913586936329 ) ) ;
#7931 = ORIENTED_EDGE ( 'NONE', *, *, #7418, .T. ) ;
#7932 = AXIS2_PLACEMENT_3D ( 'NONE', #8367, #8497, #6433 ) ;
#7933 = VERTEX_POINT ( 'NONE', #6963 ) ;
#7934 = ADVANCED_FACE ( 'NONE', ( #594 ), #9142, .T. ) ;
#7935 = DIRECTION ( 'NONE',  ( 0.000000000000000000, 0.000000000000000000, -1.000000000000000000 ) ) ;
#7936 = CARTESIAN_POINT ( 'NONE',  ( -2.692658234374996518, -27.31770833299193413, 4.663820869356208654 ) ) ;
#7937 = CARTESIAN_POINT ( 'NONE',  ( -0.01814118441313417734, -5.750659073900639129, -4.000000000000000000 ) ) ;
#7938 = CARTESIAN_POINT ( 'NONE',  ( 1.406733260263385521, -29.36383544963257108, 5.250000000000006217 ) ) ;
#7939 = ORIENTED_EDGE ( 'NONE', *, *, #8173, .T. ) ;
#7940 = CARTESIAN_POINT ( 'NONE',  ( -2.624999999999996891, -27.89583333265053255, 4.546633369868304797 ) ) ;
#7941 = LINE ( 'NONE', #3014, #10 ) ;
#7942 = CARTESIAN_POINT ( 'NONE',  ( -5.385316468750000141, -28.35937499965860198, 0.000000000000000000 ) ) ;
#7943 = CARTESIAN_POINT ( 'NONE',  ( -5.114683531250000748, -27.48437500034139802, -6.263680815196995234E-16 ) ) ;
#7944 = CARTESIAN_POINT ( 'NONE',  ( 3.507514324621465285, -2.749340926099361315, -1.431606283892619125 ) ) ;
#7945 = CARTESIAN_POINT ( 'NONE',  ( -5.385316468750001029, -27.09895833299193413, -3.109213912904136734 ) ) ;
#7946 = CARTESIAN_POINT ( 'NONE',  ( -3.000000000000000444, -8.249340926099360871, -0.01814118441320822922 ) ) ;
#7947 = CARTESIAN_POINT ( 'NONE',  ( -5.249999999999999112, -29.45833333265053611, -3.031088913245534755 ) ) ;
#7948 = CARTESIAN_POINT ( 'NONE',  ( -4.007514324621467949, -3.549340926099360694, 1.638713065079161924 ) ) ;
#7949 = CARTESIAN_POINT ( 'NONE',  ( -5.250000000000000000, -28.45833333265053611, -3.031088913245534755 ) ) ;
#7950 = DIRECTION ( 'NONE',  ( -0.000000000000000000, 1.000000000000000000, -0.000000000000000000 ) ) ;
#7951 = CYLINDRICAL_SURFACE ( 'NONE', #8171, 2.500000000000000000 ) ;
#7952 = ORIENTED_EDGE ( 'NONE', *, *, #4703, .T. ) ;
#7953 = CARTESIAN_POINT ( 'NONE',  ( -3.807688866302469071E-16, -27.64062499965859843, -6.218427825808274356 ) ) ;
#7954 = EDGE_CURVE ( 'NONE', #3636, #1967, #718, .T. ) ;
#7955 = CARTESIAN_POINT ( 'NONE',  ( 0.000000000000000000, -27.00000000000000000, -6.250000000000000000 ) ) ;
#7956 = ORIENTED_EDGE ( 'NONE', *, *, #4233, .F. ) ;
#7957 = CARTESIAN_POINT ( 'NONE',  ( 5.385316468749999252, -27.18229166632526628, -3.109213912904139399 ) ) ;
#7958 = CARTESIAN_POINT ( 'NONE',  ( 3.000000000000000444, -6.950659073900640195, -0.01814118441314496039 ) ) ;
#7959 = ORIENTED_EDGE ( 'NONE', *, *, #4485, .F. ) ;
#7960 = CARTESIAN_POINT ( 'NONE',  ( 2.624999999999996891, -29.54166666666666430, 4.546633369868304797 ) ) ;
#7961 = CARTESIAN_POINT ( 'NONE',  ( -2.557341765625002594, -28.25520833367473017, 4.429445870380399164 ) ) ;
#7962 = CARTESIAN_POINT ( 'NONE',  ( -5.249999999999999112, -27.22916666666666430, 3.031088913245538308 ) ) ;
#7963 = CARTESIAN_POINT ( 'NONE',  ( 5.114683531250000748, -26.89062500034139802, 0.000000000000000000 ) ) ;
#7964 = CARTESIAN_POINT ( 'NONE',  ( -2.462045979635576920, -6.449340926099361937, -2.487701488670255756 ) ) ;
#7965 = APPLICATION_CONTEXT ( 'automotive_design' ) ;
#7966 = DIRECTION ( 'NONE',  ( 0.000000000000000000, -0.000000000000000000, 1.000000000000000000 ) ) ;
#7967 = CARTESIAN_POINT ( 'NONE',  ( -5.249999999999999112, -27.77083333333333215, -3.031088913245534755 ) ) ;
#7968 = CARTESIAN_POINT ( 'NONE',  ( -1.406733260263393293, -29.70758545099816317, -5.250000000000000000 ) ) ;
#7969 = FACE_OUTER_BOUND ( 'NONE', #3177, .T. ) ;
#7970 = EDGE_LOOP ( 'NONE', ( #788, #715, #7772, #6773 ) ) ;
#7971 = CARTESIAN_POINT ( 'NONE',  ( 0.000000000000000000, -27.00000000000000000, -5.250000000000000000 ) ) ;
#7972 = CARTESIAN_POINT ( 'NONE',  ( -1.084901341431563923E-15, -28.92187500034139447, 5.905927827173866440 ) ) ;
#7973 = ORIENTED_EDGE ( 'NONE', *, *, #7856, .T. ) ;
#7974 = CARTESIAN_POINT ( 'NONE',  ( 2.625000000000002220, -29.66666666666666785, 4.546633369868302132 ) ) ;
#7975 = CARTESIAN_POINT ( 'NONE',  ( 2.625000000000002220, -28.16666666666666785, 4.546633369868302132 ) ) ;
#7976 = CARTESIAN_POINT ( 'NONE',  ( -4.007514324621431534, -6.050659073900639839, -1.638713065079248521 ) ) ;
#7977 =( NAMED_UNIT ( * ) PLANE_ANGLE_UNIT ( ) SI_UNIT ( $, .RADIAN. ) );
#7978 = ORIENTED_EDGE ( 'NONE', *, *, #2365, .F. ) ;
#7979 = ADVANCED_FACE ( 'NONE', ( #4175 ), #7892, .T. ) ;
#7980 = LINE ( 'NONE', #255, #1786 ) ;
#7981 = CARTESIAN_POINT ( 'NONE',  ( -5.385316468749998364, -28.58854166632526983, 3.109213912904140287 ) ) ;
#7982 = CARTESIAN_POINT ( 'NONE',  ( 5.114683531249998971, -27.63020833367473017, 2.952963913586936329 ) ) ;
#7983 = LINE ( 'NONE', #4407, #6726 ) ;
#7984 = CARTESIAN_POINT ( 'NONE',  ( 5.385316468749999252, -27.43229166632526628, -3.109213912904138954 ) ) ;
#7985 = CARTESIAN_POINT ( 'NONE',  ( -2.992485675378564469, -4.650659073900640372, 1.260781871532430820 ) ) ;
#7986 = CARTESIAN_POINT ( 'NONE',  ( -5.250000000000000000, -29.43749999931720041, 0.000000000000000000 ) ) ;
#7987 = CARTESIAN_POINT ( 'NONE',  ( 2.841254879263533262, -2.849340926099360960, -2.815599370228847320 ) ) ;
#7988 = EDGE_CURVE ( 'NONE', #2117, #1943, #5651, .T. ) ;
#7989 = CARTESIAN_POINT ( 'NONE',  ( -5.250000000000000000, -27.95833333265052900, -3.031088913245534755 ) ) ;
#7990 = CARTESIAN_POINT ( 'NONE',  ( -3.500000000000000000, 0.000000000000000000, -3.665958595716611867E-14 ) ) ;
#7991 = CARTESIAN_POINT ( 'NONE',  ( 3.500000000000000000, -1.049340926099360916, 0.01814118441321387054 ) ) ;
#7992 = EDGE_CURVE ( 'NONE', #1967, #6715, #8317, .T. ) ;
#7993 =( BOUNDED_CURVE ( )  B_SPLINE_CURVE ( 2, ( #3329, #6808, #3373, #8938, #1934 ),
 .UNSPECIFIED., .F., .F. ) 
 B_SPLINE_CURVE_WITH_KNOTS ( ( 3, 2, 3 ),
 ( 0.9791666666666667407, 0.9861111111111111605, 1.000000000000000000 ),
 .UNSPECIFIED. ) 
 CURVE ( )  GEOMETRIC_REPRESENTATION_ITEM ( )  RATIONAL_B_SPLINE_CURVE ( ( 0.9330127018922192983, 0.9330127018922198534, 1.000000000000000000, 0.8660254037844387076, 1.000000000000000000 ) ) 
 REPRESENTATION_ITEM ( '' )  );
#7994 = CARTESIAN_POINT ( 'NONE',  ( 2.161402558328724325E-14, -28.99999999931720751, -5.250000000000000000 ) ) ;
#7995 = EDGE_LOOP ( 'NONE', ( #7224, #736, #1150, #8618 ) ) ;
#7996 = CARTESIAN_POINT ( 'NONE',  ( 0.000000000000000000, 0.000000000000000000, 0.000000000000000000 ) ) ;
#7997 = CARTESIAN_POINT ( 'NONE',  ( -3.807688866302469071E-16, -28.64062499965860198, -6.218427825808274356 ) ) ;
#7998 = CARTESIAN_POINT ( 'NONE',  ( -3.992485675378532939, -1.749340926099360871, -1.674995433905601683 ) ) ;
#7999 = CYLINDRICAL_SURFACE ( 'NONE', #5176, 5.250000000000000000 ) ;
#8000 = VERTEX_POINT ( 'NONE', #70 ) ;
#8001 = CARTESIAN_POINT ( 'NONE',  ( 1.224499502706142273, -7.250659073900640905, -3.007514324621435531 ) ) ;
#8002 = VERTEX_POINT ( 'NONE', #6346 ) ;
#8003 = CARTESIAN_POINT ( 'NONE',  ( -2.625000000000002220, -27.33333333333333215, 4.546633369868302132 ) ) ;
#8004 = CIRCLE ( 'NONE', #6663, 2.500000000000000444 ) ;
#8005 = APPLICATION_CONTEXT ( 'automotive_design' ) ;
#8006 = CARTESIAN_POINT ( 'NONE',  ( 5.114683531249998971, -28.44270833367473017, 2.952963913586936329 ) ) ;
#8007 = CARTESIAN_POINT ( 'NONE',  ( -1.406733260263394847, -29.45758545099816317, -5.250000000000000000 ) ) ;
#8008 = CARTESIAN_POINT ( 'NONE',  ( -5.385316468750000141, -27.07812499965860198, 0.000000000000000000 ) ) ;
#8009 = CARTESIAN_POINT ( 'NONE',  ( 2.487701488670255756, -6.049340926099361582, -2.462045979635577364 ) ) ;
#8010 = PLANE ( 'NONE',  #2075 ) ;
#8011 = CARTESIAN_POINT ( 'NONE',  ( 1.406733260263394625, -28.69866454968462577, -5.250000000000000000 ) ) ;
#8012 = CARTESIAN_POINT ( 'NONE',  ( 5.114683531250000748, -28.67187500034139802, 0.000000000000000000 ) ) ;
#8013 = CARTESIAN_POINT ( 'NONE',  ( 1.406733260263405061, -28.22991455036742181, -5.249999999999994671 ) ) ;
#8014 = VERTEX_POINT ( 'NONE', #7144 ) ;
#8015 = AXIS2_PLACEMENT_3D ( 'NONE', #2908, #4811, #7656 ) ;
#8016 = CARTESIAN_POINT ( 'NONE',  ( -1.406733260263387963, -28.70758545099816672, -5.250000000000001776 ) ) ;
#8017 = CARTESIAN_POINT ( 'NONE',  ( -1.000000000000000000, -35.00000000000000000, -3.048902179152658931 ) ) ;
#8018 = CARTESIAN_POINT ( 'NONE',  ( 5.114683531250000748, -28.85937500034139802, 0.000000000000000000 ) ) ;
#8019 = AXIS2_PLACEMENT_3D ( 'NONE', #8494, #4981, #4214 ) ;
#8020 = ORIENTED_EDGE ( 'NONE', *, *, #8892, .F. ) ;
#8021 = CARTESIAN_POINT ( 'NONE',  ( 0.000000000000000000, -20.00000000000000000, 0.000000000000000000 ) ) ;
#8022 = CARTESIAN_POINT ( 'NONE',  ( -1.674995433905516196, -4.250659073900640017, -3.992485675378566690 ) ) ;
#8023 = DIRECTION ( 'NONE',  ( 0.000000000000000000, 0.000000000000000000, -1.000000000000000000 ) ) ;
#8024 = ORIENTED_EDGE ( 'NONE', *, *, #901, .T. ) ;
#8025 = PRODUCT_RELATED_PRODUCT_CATEGORY ( 'part', '', ( #8393 ) ) ;
#8026 = AXIS2_PLACEMENT_3D ( 'NONE', #130, #3670, #7771 ) ;
#8027 = CYLINDRICAL_SURFACE ( 'NONE', #2079, 5.250000000000000000 ) ;
#8028 = CARTESIAN_POINT ( 'NONE',  ( 2.624999999999996891, -28.82291666734946389, 4.546633369868304797 ) ) ;
#8029 = CARTESIAN_POINT ( 'NONE',  ( 5.385316468750001029, -27.50520833299193768, 3.109213912904135846 ) ) ;
#8030 = CARTESIAN_POINT ( 'NONE',  ( -5.114683531250000748, -26.96354166700806587, 2.952963913586931888 ) ) ;
#8031 = ORIENTED_EDGE ( 'NONE', *, *, #2513, .T. ) ;
#8032 = CARTESIAN_POINT ( 'NONE',  ( -5.385316468750001029, -27.34895833299193413, -3.109213912904136734 ) ) ;
#8033 = CARTESIAN_POINT ( 'NONE',  ( -2.134148098076932953, -4.350659073900638774, -2.108492589042352705 ) ) ;
#8034 = UNCERTAINTY_MEASURE_WITH_UNIT (LENGTH_MEASURE( 1.000000000000000082E-05 ), #8657, 'distance_accuracy_value', 'NONE');
#8035 = DIRECTION ( 'NONE',  ( 0.000000000000000000, 1.000000000000000000, 0.000000000000000000 ) ) ;
#8036 = CARTESIAN_POINT ( 'NONE',  ( -2.815599370228846876, -3.249340926099360871, -2.841254879263533262 ) ) ;
#8037 = EDGE_CURVE ( 'NONE', #2249, #154, #7708, .T. ) ;
#8038 = CARTESIAN_POINT ( 'NONE',  ( 2.624999999999998668, -27.77083333265053255, -4.546633369868303021 ) ) ;
#8039 = CARTESIAN_POINT ( 'NONE',  ( 0.000000000000000000, 0.000000000000000000, 0.000000000000000000 ) ) ;
#8040 = CARTESIAN_POINT ( 'NONE',  ( 3.500000000000000000, -4.249340926099360871, 0.01814118441321387054 ) ) ;
#8041 = EDGE_CURVE ( 'NONE', #2470, #6852, #4860, .T. ) ;
#8042 = DIRECTION ( 'NONE',  ( -0.000000000000000000, 1.000000000000000000, -0.000000000000000000 ) ) ;
#8043 = FILL_AREA_STYLE_COLOUR ( '', #5608 ) ;
#8044 = CARTESIAN_POINT ( 'NONE',  ( 2.692658234374998738, -28.16145833299193413, -4.663820869356206877 ) ) ;
#8045 = CARTESIAN_POINT ( 'NONE',  ( -4.007514324621467949, -3.549340926099360694, 1.638713065079161924 ) ) ;
#8046 = CYLINDRICAL_SURFACE ( 'NONE', #8312, 4.250000000000000000 ) ;
#8047 = ORIENTED_EDGE ( 'NONE', *, *, #6056, .T. ) ;
#8048 = CARTESIAN_POINT ( 'NONE',  ( -5.385316468749998364, -28.30729166632526628, 3.109213912904140287 ) ) ;
#8049 = CARTESIAN_POINT ( 'NONE',  ( 1.431606283892694842, -0.8506590739006389956, -3.507514324621434199 ) ) ;
#8050 = VERTEX_POINT ( 'NONE', #2037 ) ;
#8051 = CARTESIAN_POINT ( 'NONE',  ( 5.250000000000000000, -28.47916666666666785, -3.031088913245534755 ) ) ;
#8052 = EDGE_CURVE ( 'NONE', #105, #4617, #2078, .T. ) ;
#8053 =( BOUNDED_CURVE ( )  B_SPLINE_CURVE ( 2, ( #8158, #1133, #5307, #2483, #3973, #5963, #3230, #8801, #333 ),
 .UNSPECIFIED., .F., .F. ) 
 B_SPLINE_CURVE_WITH_KNOTS ( ( 3, 2, 2, 2, 3 ),
 ( 0.3958333333333333703, 0.4027777777777777901, 0.4166666666666666852, 0.4305555555555555802, 0.4375000000000000000 ),
 .UNSPECIFIED. ) 
 CURVE ( )  GEOMETRIC_REPRESENTATION_ITEM ( )  RATIONAL_B_SPLINE_CURVE ( ( 0.9330127018922194093, 0.9330127018922196314, 1.000000000000000000, 0.8660254037844387076, 1.000000000000000000, 0.8660254037844387076, 1.000000000000000000, 0.9330127018922194093, 0.9330127018922194093 ) ) 
 REPRESENTATION_ITEM ( '' )  );
#8054 = CARTESIAN_POINT ( 'NONE',  ( -5.114683531250001636, -27.52604166700806587, 2.952963913586931444 ) ) ;
#8055 = SURFACE_STYLE_FILL_AREA ( #937 ) ;
#8056 = CARTESIAN_POINT ( 'NONE',  ( 2.625000000000002220, -27.41666666666666430, 4.546633369868302132 ) ) ;
#8057 = CARTESIAN_POINT ( 'NONE',  ( 0.000000000000000000, -9.000000000000001776, 0.000000000000000000 ) ) ;
#8058 = CARTESIAN_POINT ( 'NONE',  ( 3.507514324621465285, -2.749340926099361315, -1.431606283892619125 ) ) ;
#8059 = DIRECTION ( 'NONE',  ( 0.000000000000000000, 0.000000000000000000, 1.000000000000000000 ) ) ;
#8060 = CARTESIAN_POINT ( 'NONE',  ( -1.406733260263397289, -28.19866454968463287, 5.249999999999997335 ) ) ;
#8061 = CARTESIAN_POINT ( 'NONE',  ( -5.114683531249999859, -28.81770833367473017, -2.952963913586935440 ) ) ;
#8062 = EDGE_LOOP ( 'NONE', ( #8630, #5400, #8096, #8290 ) ) ;
#8063 = CONICAL_SURFACE ( 'NONE', #3025, 5.257453848358681014, 0.1221730476396033355 ) ;
#8064 = AXIS2_PLACEMENT_3D ( 'NONE', #1134, #2583, #8847 ) ;
#8065 = CARTESIAN_POINT ( 'NONE',  ( 0.000000000000000000, 75.00000000000000000, 0.000000000000000000 ) ) ;
#8066 = CARTESIAN_POINT ( 'NONE',  ( -1.084901341431563923E-15, -28.17187500034139447, 5.905927827173866440 ) ) ;
#8067 = EDGE_CURVE ( 'NONE', #3693, #2716, #7009, .T. ) ;
#8068 = EDGE_LOOP ( 'NONE', ( #8407, #5762 ) ) ;
#8069 = CARTESIAN_POINT ( 'NONE',  ( 5.250000000000000000, -26.78125000068279604, 0.000000000000000000 ) ) ;
#8070 = CARTESIAN_POINT ( 'NONE',  ( 1.142306659890740623E-15, -27.29687499965859843, 6.218427825808274356 ) ) ;
#8071 = CARTESIAN_POINT ( 'NONE',  ( -3.992485675378568022, -6.250659073900639129, 1.674995433905515529 ) ) ;
#8072 = AXIS2_PLACEMENT_3D ( 'NONE', #4802, #4759, #3277 ) ;
#8073 = CARTESIAN_POINT ( 'NONE',  ( -5.249999999999999112, -29.14583333333333925, -3.031088913245536975 ) ) ;
#8074 = CARTESIAN_POINT ( 'NONE',  ( 5.385316468749999252, -27.71354166632526272, -3.109213912904139399 ) ) ;
#8075 = ORIENTED_EDGE ( 'NONE', *, *, #5081, .T. ) ;
#8076 = CARTESIAN_POINT ( 'NONE',  ( -5.250000000000000888, -29.85416666666666430, 3.031088913245533423 ) ) ;
#8077 = CARTESIAN_POINT ( 'NONE',  ( 5.250000000000000000, -28.76041666734946389, -3.031088913245534755 ) ) ;
#8078 =( BOUNDED_CURVE ( )  B_SPLINE_CURVE ( 2, ( #7518, #4039, #7567, #2601, #1147, #3990, #5559, #759, #4168 ),
 .UNSPECIFIED., .F., .T. ) 
 B_SPLINE_CURVE_WITH_KNOTS ( ( 3, 2, 2, 2, 3 ),
 ( 0.1458333333333333426, 0.1527777777777777901, 0.1666666666666666574, 0.1805555555555555525, 0.1875000000000000000 ),
 .UNSPECIFIED. ) 
 CURVE ( )  GEOMETRIC_REPRESENTATION_ITEM ( )  RATIONAL_B_SPLINE_CURVE ( ( 0.9330127018922194093, 0.9330127018922194093, 1.000000000000000000, 0.8660254037844387076, 1.000000000000000000, 0.8660254037844387076, 1.000000000000000000, 0.9330127018922194093, 0.9330127018922194093 ) ) 
 REPRESENTATION_ITEM ( '' )  );
#8079 = CARTESIAN_POINT ( 'NONE',  ( 2.692658234375002735, -28.27604166632526628, 4.663820869356205101 ) ) ;
#8080 = VECTOR ( 'NONE', #1910, 1000.000000000000000 ) ;
#8081 = CARTESIAN_POINT ( 'NONE',  ( -2.557341765624999042, -27.52604166700806587, -4.429445870380400052 ) ) ;
#8082 = ORIENTED_EDGE ( 'NONE', *, *, #74, .F. ) ;
#8083 = CYLINDRICAL_SURFACE ( 'NONE', #7637, 5.250000000000000000 ) ;
#8084 = CARTESIAN_POINT ( 'NONE',  ( -2.992485675378564469, -1.450659073900639751, 1.260781871532430820 ) ) ;
#8085 = LINE ( 'NONE', #3116, #1611 ) ;
#8086 = CARTESIAN_POINT ( 'NONE',  ( -2.624999999999996891, -27.39583333265053611, 4.546633369868304797 ) ) ;
#8087 = CARTESIAN_POINT ( 'NONE',  ( 5.249999999999999112, -27.60416666666666430, -3.031088913245536975 ) ) ;
#8088 = CARTESIAN_POINT ( 'NONE',  ( -3.500000000000000000, -1.849340926099361182, -0.01814118441321344033 ) ) ;
#8089 = DIRECTION ( 'NONE',  ( 0.000000000000000000, -1.000000000000000000, 0.000000000000000000 ) ) ;
#8090 = VERTEX_POINT ( 'NONE', #3566 ) ;
#8091 = DIRECTION ( 'NONE',  ( 0.000000000000000000, 0.000000000000000000, 1.000000000000000000 ) ) ;
#8092 = CARTESIAN_POINT ( 'NONE',  ( -2.692658234375000514, -27.61979166632526628, -4.663820869356205989 ) ) ;
#8093 = B_SPLINE_CURVE_WITH_KNOTS ( 'NONE', 3,
 ( #1448, #3596, #4292, #5680 ),
 .UNSPECIFIED., .F., .F.,
 ( 4, 4 ),
 ( 0.008577873411363935718, 0.01459462325714742936 ),
 .UNSPECIFIED. ) ;
#8094 = CARTESIAN_POINT ( 'NONE',  ( 3.992485675378533383, -4.149340926099362115, 1.674995433905599462 ) ) ;
#8095 = CARTESIAN_POINT ( 'NONE',  ( -5.249999999999999112, -28.52083333333333215, -3.031088913245534755 ) ) ;
#8096 = ORIENTED_EDGE ( 'NONE', *, *, #3103, .F. ) ;
#8097 = CARTESIAN_POINT ( 'NONE',  ( 5.385316468749999252, -28.93229166632526628, -3.109213912904139399 ) ) ;
#8098 = CARTESIAN_POINT ( 'NONE',  ( -3.507514324621434199, -1.250659073900638907, -1.431606283892695064 ) ) ;
#8099 = VERTEX_POINT ( 'NONE', #7844 ) ;
#8100 = CARTESIAN_POINT ( 'NONE',  ( -5.250000000000000888, -27.60416666666666785, 3.031088913245532979 ) ) ;
#8101 = ADVANCED_FACE ( 'NONE', ( #1461, #4308 ), #676, .T. ) ;
#8102 = CARTESIAN_POINT ( 'NONE',  ( 1.431606283892694620, -0.8506590739006389956, -3.507514324621433754 ) ) ;
#8103 = ORIENTED_EDGE ( 'NONE', *, *, #4907, .T. ) ;
#8104 = FACE_OUTER_BOUND ( 'NONE', #4660, .T. ) ;
#8105 = ORIENTED_EDGE ( 'NONE', *, *, #7576, .F. ) ;
#8106 = CARTESIAN_POINT ( 'NONE',  ( -5.114683531250000748, -28.50520833367472662, -2.952963913586935440 ) ) ;
#8107 = CARTESIAN_POINT ( 'NONE',  ( 0.01814118441321408565, -4.649340926099361226, -3.500000000000000000 ) ) ;
#8108 = FACE_BOUND ( 'NONE', #7161, .T. ) ;
#8109 = CARTESIAN_POINT ( 'NONE',  ( -2.624999999999998668, -28.16666666666666785, -4.546633369868303021 ) ) ;
#8110 = CARTESIAN_POINT ( 'NONE',  ( 5.114683531249999859, -29.15104166700806232, -2.952963913586932776 ) ) ;
#8111 = CARTESIAN_POINT ( 'NONE',  ( 0.000000000000000000, -9.999999999999998224, 0.000000000000000000 ) ) ;
#8112 = ORIENTED_EDGE ( 'NONE', *, *, #8224, .F. ) ;
#8113 = EDGE_CURVE ( 'NONE', #3780, #2524, #4260, .T. ) ;
#8114 = CARTESIAN_POINT ( 'NONE',  ( 2.624999999999996891, -29.29166666666666785, 4.546633369868304797 ) ) ;
#8115 = CARTESIAN_POINT ( 'NONE',  ( 3.616337804771879580E-16, -27.04687500034139802, -5.905927827173866440 ) ) ;
#8116 = VERTEX_POINT ( 'NONE', #3610 ) ;
#8117 = CARTESIAN_POINT ( 'NONE',  ( 7.654042494670957606E-16, -27.00000000000000000, 6.250000000000000000 ) ) ;
#8118 = CARTESIAN_POINT ( 'NONE',  ( -2.692658234374996518, -28.31770833299193413, 4.663820869356208654 ) ) ;
#8119 = CARTESIAN_POINT ( 'NONE',  ( -1.674995433905516196, -7.450659073900640195, -3.992485675378566690 ) ) ;
#8120 =( LENGTH_UNIT ( ) NAMED_UNIT ( * ) SI_UNIT ( .MILLI., .METRE. ) );
#8121 = CARTESIAN_POINT ( 'NONE',  ( 2.692658234374998738, -27.69270833299193768, -4.663820869356206877 ) ) ;
#8122 = EDGE_CURVE ( 'NONE', #1844, #738, #2921, .T. ) ;
#8123 = EDGE_LOOP ( 'NONE', ( #1532, #2828 ) ) ;
#8124 = CARTESIAN_POINT ( 'NONE',  ( -1.406733260263391960, -27.88616454900183328, 5.250000000000000000 ) ) ;
#8125 = CARTESIAN_POINT ( 'NONE',  ( 5.249999999999999112, -29.55208333401613885, 3.031088913245538308 ) ) ;
#8126 = CARTESIAN_POINT ( 'NONE',  ( 2.692658234374998738, -27.44270833299193413, -4.663820869356206877 ) ) ;
#8127 = UNCERTAINTY_MEASURE_WITH_UNIT (LENGTH_MEASURE( 1.000000000000000082E-05 ), #6548, 'distance_accuracy_value', 'NONE');
#8128 = VERTEX_POINT ( 'NONE', #8583 ) ;
#8129 = APPLICATION_CONTEXT ( 'automotive_design' ) ;
#8130 = CARTESIAN_POINT ( 'NONE',  ( 5.385316468750001029, -28.72395833299193413, 3.109213912904134958 ) ) ;
#8131 = CARTESIAN_POINT ( 'NONE',  ( 3.000000000000000444, -0.5506590739006393953, -0.01814118441314496039 ) ) ;
#8132 = CARTESIAN_POINT ( 'NONE',  ( 0.000000000000000000, 75.00000000000000000, 0.000000000000000000 ) ) ;
#8133 =( BOUNDED_SURFACE ( )  B_SPLINE_SURFACE ( 1, 2, ( 
 ( #4295, #7267, #2295, #7085, #6377, #5120, #6468, #801, #8571, #6566, #4341, #4432, #199, #2200, #7177, #103, #5773, #17, #5071, #3599, #8616, #2247, #2865, #754, #7924, #4482, #2439, #8758, #7317, #5965, #8935, #1836, #1691, #3832, #288, #2533, #3232, #8110, #3975, #2389, #1087, #5170, #986, #428, #4575, #6053, #3929, #7362, #5265, #3884, #6757, #383, #5219, #8061, #1739, #3145, #3276, #7507, #8891, #6105, #8012, #7460, #5357, #6658, #8802, #4531, #7411, #8205, #1034, #6706, #1135, #1643, #4668, #943, #335, #6803, #3188, #3791, #6615, #242, #5916, #3093, #6009, #8848, #2485, #5308, #8160, #1789, #4622, #4066, #4197, #6988, #2719, #2016, #3415, #4758, #3325, #8347, #8430, #7032, #1972, #9121, #479, #7602, #1887, #9029, #6156, #4712, #3370, #6324, #2058, #8297, #1226, #6905, #2766, #1310, #4883, #5586, #7551, #529, #2584, #6201, #615, #4152, #3501, #4841, #5544, #7644, #2674, #3456, #8984, #1358, #659, #2633, #5404, #5452, #4021, #6942, #7686, #8254, #1178, #1930, #6285, #8389, #7735 ),
 ( #6856, #5501, #4801, #1272, #4110, #571, #6245, #9077, #7165, #744, #8479, #7779, #2285, #697, #2189, #4242, #8521, #7074, #4286, #5061, #7211, #2900, #7960, #6367, #7914, #9160, #4970, #4425, #8561, #836, #1536, #2149, #6413, #7867, #4379, #3681, #3542, #6, #5718, #7119, #7257, #5111, #6503, #884, #3734, #2237, #140, #1440, #7824, #2857, #3589, #2992, #52, #5673, #1584, #2809, #8653, #5629, #5011, #5815, #1489, #2103, #4926, #1401, #4333, #792, #3637, #6459, #92, #2942, #5763, #8605, #7352, #8051, #8195, #1776, #6695, #5999, #7400, #8746, #2426, #5255, #4565, #5210, #4523, #5861, #5345, #978, #6743, #1632, #3042, #3132, #5298, #324, #1023, #3824, #7497, #1823, #2519, #373, #4612, #3085, #278, #8838, #8878, #932, #1123, #4654, #6557, #3221, #1728, #1680, #6041, #3918, #188, #8100, #5955, #6649, #3873, #3178, #2474, #8701, #8149, #7450, #8794, #2332, #5161, #1075, #8003, #4470, #7308, #3781, #6607, #236, #5907, #2380, #6236, #2623, #8973, #1302, #6977, #6192, #1217, #2709, #3264 ) ),
 .UNSPECIFIED., .F., .F., .F. ) 
 B_SPLINE_SURFACE_WITH_KNOTS ( ( 2, 2 ),
 ( 3, 2, 2, 2, 2, 2, 2, 2, 2, 2, 2, 2, 2, 2, 2, 2, 2, 2, 2, 2, 2, 2, 2, 2, 2, 2, 2, 2, 2, 2, 2, 2, 2, 2, 2, 2, 2, 2, 2, 2, 2, 2, 2, 2, 2, 2, 2, 2, 2, 2, 2, 2, 2, 2, 2, 2, 2, 2, 2, 2, 2, 2, 2, 2, 2, 2, 2, 2, 2, 2, 2, 2, 3 ),
 ( 0.000000000000000000, 1.000000000000000000 ),
 ( 0.000000000000000000, 0.01388888888888888812, 0.02777777777777777624, 0.04166666666666666435, 0.05555555555555555247, 0.06944444444444444753, 0.08333333333333332871, 0.09722222222222222376, 0.1111111111111111049, 0.1250000000000000000, 0.1388888888888888951, 0.1527777777777777901, 0.1666666666666666574, 0.1805555555555555525, 0.1944444444444444475, 0.2083333333333333426, 0.2222222222222222099, 0.2361111111111111049, 0.2500000000000000000, 0.2638888888888888951, 0.2777777777777777901, 0.2916666666666666852, 0.3055555555555555802, 0.3194444444444444198, 0.3333333333333333148, 0.3472222222222222099, 0.3611111111111111049, 0.3750000000000000000, 0.3888888888888888951, 0.4027777777777777901, 0.4166666666666666852, 0.4305555555555555802, 0.4444444444444444198, 0.4583333333333333148, 0.4722222222222222099, 0.4861111111111111049, 0.5000000000000000000, 0.5138888888888888395, 0.5277777777777777901, 0.5416666666666666297, 0.5555555555555555802, 0.5694444444444444198, 0.5833333333333333703, 0.5972222222222222099, 0.6111111111111111605, 0.6250000000000000000, 0.6388888888888888395, 0.6527777777777777901, 0.6666666666666666297, 0.6805555555555555802, 0.6944444444444444198, 0.7083333333333333703, 0.7222222222222222099, 0.7361111111111111605, 0.7500000000000000000, 0.7638888888888888395, 0.7777777777777777901, 0.7916666666666666297, 0.8055555555555555802, 0.8194444444444444198, 0.8333333333333333703, 0.8472222222222222099, 0.8611111111111111605, 0.8750000000000000000, 0.8888888888888888395, 0.9027777777777777901, 0.9166666666666666297, 0.9305555555555555802, 0.9444444444444444198, 0.9583333333333333703, 0.9722222222222222099, 0.9861111111111111605, 1.000000000000000000 ),
 .UNSPECIFIED. ) 
 GEOMETRIC_REPRESENTATION_ITEM ( )  RATIONAL_B_SPLINE_SURFACE ( (
 ( 1.000000000000000000, 0.8660254037844387076, 1.000000000000000000, 0.8660254037844387076, 1.000000000000000000, 0.8660254037844387076, 1.000000000000000000, 0.8660254037844387076, 1.000000000000000000, 0.8660254037844387076, 1.000000000000000000, 0.8660254037844387076, 1.000000000000000000, 0.8660254037844387076, 1.000000000000000000, 0.8660254037844387076, 1.000000000000000000, 0.8660254037844387076, 1.000000000000000000, 0.8660254037844387076, 1.000000000000000000, 0.8660254037844387076, 1.000000000000000000, 0.8660254037844387076, 1.000000000000000000, 0.8660254037844387076, 1.000000000000000000, 0.8660254037844387076, 1.000000000000000000, 0.8660254037844387076, 1.000000000000000000, 0.8660254037844387076, 1.000000000000000000, 0.8660254037844387076, 1.000000000000000000, 0.8660254037844387076, 1.000000000000000000, 0.8660254037844387076, 1.000000000000000000, 0.8660254037844387076, 1.000000000000000000, 0.8660254037844387076, 1.000000000000000000, 0.8660254037844387076, 1.000000000000000000, 0.8660254037844387076, 1.000000000000000000, 0.8660254037844387076, 1.000000000000000000, 0.8660254037844387076, 1.000000000000000000, 0.8660254037844387076, 1.000000000000000000, 0.8660254037844387076, 1.000000000000000000, 0.8660254037844387076, 1.000000000000000000, 0.8660254037844387076, 1.000000000000000000, 0.8660254037844387076, 1.000000000000000000, 0.8660254037844387076, 1.000000000000000000, 0.8660254037844387076, 1.000000000000000000, 0.8660254037844387076, 1.000000000000000000, 0.8660254037844387076, 1.000000000000000000, 0.8660254037844387076, 1.000000000000000000, 0.8660254037844387076, 1.000000000000000000, 0.8660254037844387076, 1.000000000000000000, 0.8660254037844387076, 1.000000000000000000, 0.8660254037844387076, 1.000000000000000000, 0.8660254037844387076, 1.000000000000000000, 0.8660254037844387076, 1.000000000000000000, 0.8660254037844387076, 1.000000000000000000, 0.8660254037844387076, 1.000000000000000000, 0.8660254037844387076, 1.000000000000000000, 0.8660254037844387076, 1.000000000000000000, 0.8660254037844387076, 1.000000000000000000, 0.8660254037844387076, 1.000000000000000000, 0.8660254037844387076, 1.000000000000000000, 0.8660254037844387076, 1.000000000000000000, 0.8660254037844387076, 1.000000000000000000, 0.8660254037844387076, 1.000000000000000000, 0.8660254037844387076, 1.000000000000000000, 0.8660254037844387076, 1.000000000000000000, 0.8660254037844387076, 1.000000000000000000, 0.8660254037844387076, 1.000000000000000000, 0.8660254037844387076, 1.000000000000000000, 0.8660254037844387076, 1.000000000000000000, 0.8660254037844387076, 1.000000000000000000, 0.8660254037844387076, 1.000000000000000000, 0.8660254037844387076, 1.000000000000000000, 0.8660254037844387076, 1.000000000000000000, 0.8660254037844387076, 1.000000000000000000, 0.8660254037844387076, 1.000000000000000000, 0.8660254037844387076, 1.000000000000000000, 0.8660254037844387076, 1.000000000000000000, 0.8660254037844387076, 1.000000000000000000, 0.8660254037844387076, 1.000000000000000000, 0.8660254037844387076, 1.000000000000000000, 0.8660254037844387076, 1.000000000000000000, 0.8660254037844387076, 1.000000000000000000, 0.8660254037844387076, 1.000000000000000000, 0.8660254037844387076, 1.000000000000000000),
 ( 1.000000000000000000, 0.8660254037844387076, 1.000000000000000000, 0.8660254037844387076, 1.000000000000000000, 0.8660254037844387076, 1.000000000000000000, 0.8660254037844387076, 1.000000000000000000, 0.8660254037844387076, 1.000000000000000000, 0.8660254037844387076, 1.000000000000000000, 0.8660254037844387076, 1.000000000000000000, 0.8660254037844387076, 1.000000000000000000, 0.8660254037844387076, 1.000000000000000000, 0.8660254037844387076, 1.000000000000000000, 0.8660254037844387076, 1.000000000000000000, 0.8660254037844387076, 1.000000000000000000, 0.8660254037844387076, 1.000000000000000000, 0.8660254037844387076, 1.000000000000000000, 0.8660254037844387076, 1.000000000000000000, 0.8660254037844387076, 1.000000000000000000, 0.8660254037844387076, 1.000000000000000000, 0.8660254037844387076, 1.000000000000000000, 0.8660254037844387076, 1.000000000000000000, 0.8660254037844387076, 1.000000000000000000, 0.8660254037844387076, 1.000000000000000000, 0.8660254037844387076, 1.000000000000000000, 0.8660254037844387076, 1.000000000000000000, 0.8660254037844387076, 1.000000000000000000, 0.8660254037844387076, 1.000000000000000000, 0.8660254037844387076, 1.000000000000000000, 0.8660254037844387076, 1.000000000000000000, 0.8660254037844387076, 1.000000000000000000, 0.8660254037844387076, 1.000000000000000000, 0.8660254037844387076, 1.000000000000000000, 0.8660254037844387076, 1.000000000000000000, 0.8660254037844387076, 1.000000000000000000, 0.8660254037844387076, 1.000000000000000000, 0.8660254037844387076, 1.000000000000000000, 0.8660254037844387076, 1.000000000000000000, 0.8660254037844387076, 1.000000000000000000, 0.8660254037844387076, 1.000000000000000000, 0.8660254037844387076, 1.000000000000000000, 0.8660254037844387076, 1.000000000000000000, 0.8660254037844387076, 1.000000000000000000, 0.8660254037844387076, 1.000000000000000000, 0.8660254037844387076, 1.000000000000000000, 0.8660254037844387076, 1.000000000000000000, 0.8660254037844387076, 1.000000000000000000, 0.8660254037844387076, 1.000000000000000000, 0.8660254037844387076, 1.000000000000000000, 0.8660254037844387076, 1.000000000000000000, 0.8660254037844387076, 1.000000000000000000, 0.8660254037844387076, 1.000000000000000000, 0.8660254037844387076, 1.000000000000000000, 0.8660254037844387076, 1.000000000000000000, 0.8660254037844387076, 1.000000000000000000, 0.8660254037844387076, 1.000000000000000000, 0.8660254037844387076, 1.000000000000000000, 0.8660254037844387076, 1.000000000000000000, 0.8660254037844387076, 1.000000000000000000, 0.8660254037844387076, 1.000000000000000000, 0.8660254037844387076, 1.000000000000000000, 0.8660254037844387076, 1.000000000000000000, 0.8660254037844387076, 1.000000000000000000, 0.8660254037844387076, 1.000000000000000000, 0.8660254037844387076, 1.000000000000000000, 0.8660254037844387076, 1.000000000000000000, 0.8660254037844387076, 1.000000000000000000, 0.8660254037844387076, 1.000000000000000000, 0.8660254037844387076, 1.000000000000000000, 0.8660254037844387076, 1.000000000000000000, 0.8660254037844387076, 1.000000000000000000, 0.8660254037844387076, 1.000000000000000000, 0.8660254037844387076, 1.000000000000000000, 0.8660254037844387076, 1.000000000000000000, 0.8660254037844387076, 1.000000000000000000) ) ) 
 REPRESENTATION_ITEM ( '' )  SURFACE ( )  );
#8134 = PRESENTATION_LAYER_ASSIGNMENT (  '', '', ( #5742 ) ) ;
#8135 = CARTESIAN_POINT ( 'NONE',  ( 5.250000000000000888, -27.33333333265053611, 3.031088913245532979 ) ) ;
#8136 = CARTESIAN_POINT ( 'NONE',  ( -3.500000000000000000, 0.000000000000000000, -3.665958595716611867E-14 ) ) ;
#8137 = CARTESIAN_POINT ( 'NONE',  ( -2.487701488670255312, -5.249340926099360871, 2.462045979635577808 ) ) ;
#8138 = CARTESIAN_POINT ( 'NONE',  ( 0.000000000000000000, 1.000000000000000000, -3.999999999999999112 ) ) ;
#8139 = VERTEX_POINT ( 'NONE', #2211 ) ;
#8140 = DIRECTION ( 'NONE',  ( 0.000000000000000000, 0.000000000000000000, 1.000000000000000000 ) ) ;
#8141 = CARTESIAN_POINT ( 'NONE',  ( -5.385316468749998364, -28.80729166632526983, 3.109213912904140287 ) ) ;
#8142 = EDGE_CURVE ( 'NONE', #627, #7705, #2610, .T. ) ;
#8143 = CARTESIAN_POINT ( 'NONE',  ( 4.000000000000000000, -2.649340926099360782, 0.01814118441321914063 ) ) ;
#8144 = CARTESIAN_POINT ( 'NONE',  ( 2.033577675846918216E-14, -27.31250000000000000, 5.250000000000000888 ) ) ;
#8145 = VERTEX_POINT ( 'NONE', #7229 ) ;
#8146 = CARTESIAN_POINT ( 'NONE',  ( 1.142306659890740623E-15, -27.76562499965860198, 6.218427825808274356 ) ) ;
#8147 = CARTESIAN_POINT ( 'NONE',  ( -3.500000000000000000, -6.150659073900639484, 0.01814118441314012051 ) ) ;
#8148 = ORIENTED_EDGE ( 'NONE', *, *, #3135, .F. ) ;
#8149 = CARTESIAN_POINT ( 'NONE',  ( 2.625000000000000444, -27.45833333333333215, -4.546633369868303021 ) ) ;
#8150 = CARTESIAN_POINT ( 'NONE',  ( 3.507514324621434199, -2.050659073900638951, 1.431606283892693066 ) ) ;
#8151 = ORIENTED_EDGE ( 'NONE', *, *, #6449, .F. ) ;
#8152 =( NAMED_UNIT ( * ) SI_UNIT ( $, .STERADIAN. ) SOLID_ANGLE_UNIT ( ) );
#8153 = CARTESIAN_POINT ( 'NONE',  ( -5.114683531250000748, -27.02604166700806587, 2.952963913586931888 ) ) ;
#8154 = EDGE_LOOP ( 'NONE', ( #495, #5057, #8082, #6144 ) ) ;
#8155 = VECTOR ( 'NONE', #7788, 1000.000000000000000 ) ;
#8156 = CARTESIAN_POINT ( 'NONE',  ( -5.114683531250000748, -29.50520833367472662, -2.952963913586935440 ) ) ;
#8157 = CARTESIAN_POINT ( 'NONE',  ( -2.134148098076978251, -5.249340926099361759, 2.108492589042307408 ) ) ;
#8158 = CARTESIAN_POINT ( 'NONE',  ( 9.180150650966086169E-15, -28.59375000068279959, 5.250000000000000000 ) ) ;
#8159 = CARTESIAN_POINT ( 'NONE',  ( 0.000000000000000000, -50.00000000000000000, -3.794308781941904574 ) ) ;
#8160 = CARTESIAN_POINT ( 'NONE',  ( 2.557341765625000818, -28.13020833367473017, -4.429445870380400052 ) ) ;
#8161 =( NAMED_UNIT ( * ) SI_UNIT ( $, .STERADIAN. ) SOLID_ANGLE_UNIT ( ) );
#8162 = CARTESIAN_POINT ( 'NONE',  ( 2.625000000000000444, -29.20833333333333215, -4.546633369868303021 ) ) ;
#8163 = FACE_OUTER_BOUND ( 'NONE', #7328, .T. ) ;
#8164 = AXIS2_PLACEMENT_3D ( 'NONE', #7524, #7479, #1862 ) ;
#8165 = PRODUCT_DEFINITION_SHAPE ( 'NONE', 'NONE',  #9190 ) ;
#8166 = ORIENTED_EDGE ( 'NONE', *, *, #1125, .T. ) ;
#8167 = DIRECTION ( 'NONE',  ( 0.000000000000000000, 0.000000000000000000, -1.000000000000000000 ) ) ;
#8168 = CARTESIAN_POINT ( 'NONE',  ( 5.385316468750001029, -28.25520833299193413, 3.109213912904134958 ) ) ;
#8169 = CARTESIAN_POINT ( 'NONE',  ( 0.000000000000000000, -30.00000000000000000, 0.000000000000000000 ) ) ;
#8170 = CARTESIAN_POINT ( 'NONE',  ( 5.385316468750000141, -29.73437499965859843, -6.595110575850215044E-16 ) ) ;
#8171 = AXIS2_PLACEMENT_3D ( 'NONE', #3167, #8042, #8785 ) ;
#8172 = ORIENTED_EDGE ( 'NONE', *, *, #6696, .F. ) ;
#8173 = EDGE_CURVE ( 'NONE', #2212, #3243, #2291, .T. ) ;
#8174=STYLED_ITEM('',(#9239),#2148);
#8175 = CARTESIAN_POINT ( 'NONE',  ( 0.000000000000000000, -30.00000000000000000, 0.000000000000000000 ) ) ;
#8176 = CARTESIAN_POINT ( 'NONE',  ( 2.624999999999996891, -27.57291666734946389, 4.546633369868304797 ) ) ;
#8177 = CARTESIAN_POINT ( 'NONE',  ( -5.385316468749998364, -29.58854166632527694, 3.109213912904140287 ) ) ;
#8178 = VERTEX_POINT ( 'NONE', #3703 ) ;
#8179 = CARTESIAN_POINT ( 'NONE',  ( 5.385316468750000141, -27.70312499965860198, -6.595110575850215044E-16 ) ) ;
#8180 = CARTESIAN_POINT ( 'NONE',  ( -3.500000000000000000, -1.350659073900638996, 0.01814118441314012051 ) ) ;
#8181 = CARTESIAN_POINT ( 'NONE',  ( 0.000000000000000000, -20.00000000000000000, 0.000000000000000000 ) ) ;
#8182 = CARTESIAN_POINT ( 'NONE',  ( -1.406733260263387963, -28.92633545031537068, -5.250000000000001776 ) ) ;
#8183 = CARTESIAN_POINT ( 'NONE',  ( -9.180150650966086169E-15, -28.37499999931720041, 5.250000000000000000 ) ) ;
#8184 = CARTESIAN_POINT ( 'NONE',  ( 0.000000000000000000, -27.00000000000000000, 0.000000000000000000 ) ) ;
#8185 = CIRCLE ( 'NONE', #1487, 6.250000000000000000 ) ;
#8186 = DIRECTION ( 'NONE',  ( -0.000000000000000000, 1.000000000000000000, -0.000000000000000000 ) ) ;
#8187 = CARTESIAN_POINT ( 'NONE',  ( 2.624999999999996891, -27.79166666666666430, 4.546633369868304797 ) ) ;
#8188 = CARTESIAN_POINT ( 'NONE',  ( 5.385316468749999252, -29.68229166632526983, -3.109213912904139399 ) ) ;
#8189 = CARTESIAN_POINT ( 'NONE',  ( 4.007514324621469726, -5.949340926099362825, -1.638713065079161257 ) ) ;
#8190 = CARTESIAN_POINT ( 'NONE',  ( -6.972266317189433020E-16, -29.06249999999999645, -5.249999999999999112 ) ) ;
#8191 = CARTESIAN_POINT ( 'NONE',  ( -3.807688866302469071E-16, -28.64062499965860198, -6.218427825808274356 ) ) ;
#8192 = CARTESIAN_POINT ( 'NONE',  ( -1.467888652718973619, -4.250659073900639129, -3.492485675378565801 ) ) ;
#8193 = CIRCLE ( 'NONE', #4180, 3.048902179152658931 ) ;
#8194 = ORIENTED_EDGE ( 'NONE', *, *, #2445, .F. ) ;
#8195 = CARTESIAN_POINT ( 'NONE',  ( 2.625000000000000444, -28.45833333333333215, -4.546633369868303021 ) ) ;
#8196 = FACE_OUTER_BOUND ( 'NONE', #4424, .T. ) ;
#8197 = CARTESIAN_POINT ( 'NONE',  ( 2.487701488670203354, -1.950659073900639084, 2.462045979635629323 ) ) ;
#8198 = ORIENTED_EDGE ( 'NONE', *, *, #8471, .F. ) ;
#8199 = CARTESIAN_POINT ( 'NONE',  ( 2.624999999999998668, -28.58333333333333215, -4.546633369868303021 ) ) ;
#8200 = PRODUCT_RELATED_PRODUCT_CATEGORY ( 'part', '', ( #691 ) ) ;
#8201 = VERTEX_POINT ( 'NONE', #5085 ) ;
#8202 = CARTESIAN_POINT ( 'NONE',  ( -2.557341765625002594, -28.94270833367473017, 4.429445870380399164 ) ) ;
#8203 = CARTESIAN_POINT ( 'NONE',  ( -3.007514324621463508, -0.3493409260993614596, 1.224499502706077658 ) ) ;
#8204 = CARTESIAN_POINT ( 'NONE',  ( -5.250000000000000888, -28.10416666666666785, 3.031088913245533423 ) ) ;
#8205 = CARTESIAN_POINT ( 'NONE',  ( -5.114683531250000748, -28.52604166700806587, 2.952963913586931888 ) ) ;
#8206 = CARTESIAN_POINT ( 'NONE',  ( -1.975475456537005874E-15, -29.31250000000000000, 5.249999999999999112 ) ) ;
#8207 = CARTESIAN_POINT ( 'NONE',  ( -5.249999999999999112, -27.92708333401612819, -3.031088913245536975 ) ) ;
#8208 = CARTESIAN_POINT ( 'NONE',  ( 5.114683531250000748, -27.35937500034139802, 0.000000000000000000 ) ) ;
#8209 = MANIFOLD_SOLID_BREP ( 'Cut-Extrude1', #5494 ) ;
#8210 = ORIENTED_EDGE ( 'NONE', *, *, #8113, .F. ) ;
#8211 = CARTESIAN_POINT ( 'NONE',  ( 5.204748896376250699E-16, -30.00000000000000000, -4.250000000000000000 ) ) ;
#8212 = ADVANCED_FACE ( 'NONE', ( #5786 ), #4593, .F. ) ;
#8213 = CARTESIAN_POINT ( 'NONE',  ( 1.142306659890740623E-15, -28.54687499965860198, 6.218427825808274356 ) ) ;
#8214 = B_SPLINE_CURVE_WITH_KNOTS ( 'NONE', 3,
 ( #1466, #8586, #4312, #8413 ),
 .UNSPECIFIED., .F., .F.,
 ( 4, 4 ),
 ( 0.008577873411363935718, 0.01459462325714742936 ),
 .UNSPECIFIED. ) ;
#8215 = CARTESIAN_POINT ( 'NONE',  ( 2.692658234375002735, -29.77604166632526983, 4.663820869356205101 ) ) ;
#8216 = CARTESIAN_POINT ( 'NONE',  ( 0.000000000000000000, 73.00000000000001421, 0.000000000000000000 ) ) ;
#8217 = CARTESIAN_POINT ( 'NONE',  ( 5.385316468749999252, -29.96354166632526628, -3.109213912904139399 ) ) ;
#8218 = CARTESIAN_POINT ( 'NONE',  ( 2.487701488670255756, -2.849340926099361404, -2.462045979635577364 ) ) ;
#8219 = CIRCLE ( 'NONE', #3469, 5.250000000000000000 ) ;
#8220 = VERTEX_POINT ( 'NONE', #2450 ) ;
#8221 = CARTESIAN_POINT ( 'NONE',  ( 7.654042494670957606E-16, -30.00000000000000000, 6.250000000000000000 ) ) ;
#8222 = CARTESIAN_POINT ( 'NONE',  ( 5.250000000000000000, -28.53125000068279604, 0.000000000000000000 ) ) ;
#8223 = CARTESIAN_POINT ( 'NONE',  ( -5.385316468750001029, -29.13020833299193058, -3.109213912904136734 ) ) ;
#8224 = EDGE_CURVE ( 'NONE', #4653, #4009, #4356, .T. ) ;
#8225 = CIRCLE ( 'NONE', #5836, 5.750000000000000000 ) ;
#8226 = VERTEX_POINT ( 'NONE', #5837 ) ;
#8227 = CARTESIAN_POINT ( 'NONE',  ( 5.385316468750000141, -28.70312499965860198, -6.595110575850215044E-16 ) ) ;
#8228 = CARTESIAN_POINT ( 'NONE',  ( -2.462045979635629323, -1.550659073900639173, 2.487701488670203798 ) ) ;
#8229 = CARTESIAN_POINT ( 'NONE',  ( 0.000000000000000000, 73.00000000000001421, 0.000000000000000000 ) ) ;
#8230 = AXIS2_PLACEMENT_3D ( 'NONE', #3253, #5527, #7669 ) ;
#8231 = AXIS2_PLACEMENT_3D ( 'NONE', #1473, #4316, #6444 ) ;
#8232 = DIRECTION ( 'NONE',  ( 0.000000000000000000, 1.000000000000000000, 0.000000000000000000 ) ) ;
#8233 = CARTESIAN_POINT ( 'NONE',  ( 2.625000000000002220, -27.41666666666666430, 4.546633369868302132 ) ) ;
#8234 = CARTESIAN_POINT ( 'NONE',  ( 5.114683531249999859, -29.33854166700805877, -2.952963913586932776 ) ) ;
#8235 = VERTEX_POINT ( 'NONE', #115 ) ;
#8236 = LINE ( 'NONE', #1211, #3627 ) ;
#8237 = CARTESIAN_POINT ( 'NONE',  ( 3.492485675378536047, -5.749340926099363536, 1.467888652719046672 ) ) ;
#8238 = AXIS2_PLACEMENT_3D ( 'NONE', #8989, #5314, #297 ) ;
#8239 = CARTESIAN_POINT ( 'NONE',  ( 0.000000000000000000, -30.00000000000000000, 4.250000000000000000 ) ) ;
#8240 = CARTESIAN_POINT ( 'NONE',  ( -5.385316468749998364, -28.80729166632526983, 3.109213912904140287 ) ) ;
#8241 = CARTESIAN_POINT ( 'NONE',  ( -3.500000000000000000, -7.750659073900639129, 0.01814118441314012051 ) ) ;
#8242 = ORIENTED_EDGE ( 'NONE', *, *, #6612, .F. ) ;
#8243 = CARTESIAN_POINT ( 'NONE',  ( -1.975475456537005874E-15, -29.06249999999999645, 5.250000000000000000 ) ) ;
#8244 = CARTESIAN_POINT ( 'NONE',  ( 3.673940397442060361E-16, 73.00000000000001421, 3.000000000000000444 ) ) ;
#8245 = CARTESIAN_POINT ( 'NONE',  ( -1.467888652718973841, -4.250659073900638241, -3.492485675378565801 ) ) ;
#8246 = EDGE_CURVE ( 'NONE', #4614, #6499, #4497, .T. ) ;
#8247 = ORIENTED_EDGE ( 'NONE', *, *, #8371, .T. ) ;
#8248 =( NAMED_UNIT ( * ) PLANE_ANGLE_UNIT ( ) SI_UNIT ( $, .RADIAN. ) );
#8249 = CARTESIAN_POINT ( 'NONE',  ( -2.625000000000000444, -29.04166666666666785, -4.546633369868303021 ) ) ;
#8250 = ORIENTED_EDGE ( 'NONE', *, *, #5006, .F. ) ;
#8251 = CARTESIAN_POINT ( 'NONE',  ( 2.557341765624996821, -29.65104166700806232, 4.429445870380401828 ) ) ;
#8252 = CARTESIAN_POINT ( 'NONE',  ( 0.01814118441320878086, -3.049340926099361138, -3.000000000000000444 ) ) ;
#8253 = CARTESIAN_POINT ( 'NONE',  ( 0.000000000000000000, -30.00000000000000000, 0.000000000000000000 ) ) ;
#8254 = CARTESIAN_POINT ( 'NONE',  ( -5.114683531250000748, -27.02604166700806587, 2.952963913586931888 ) ) ;
#8255 = PRESENTATION_STYLE_ASSIGNMENT (( #3233 ) ) ;
#8256 = DIRECTION ( 'NONE',  ( 0.000000000000000000, 0.000000000000000000, 1.000000000000000000 ) ) ;
#8257 = CARTESIAN_POINT ( 'NONE',  ( -1.084901341431563923E-15, -27.67187500034140157, 5.905927827173866440 ) ) ;
#8258 = FACE_OUTER_BOUND ( 'NONE', #2406, .T. ) ;
#8259 = CARTESIAN_POINT ( 'NONE',  ( 3.616337804771879580E-16, -29.35937500034139802, -5.905927827173866440 ) ) ;
#8260 = CARTESIAN_POINT ( 'NONE',  ( 1.000000000000000000, -20.00000000000000000, 1.118033988749894680 ) ) ;
#8261 = CARTESIAN_POINT ( 'NONE',  ( -5.385316468750001029, -29.38020833299193413, -3.109213912904136734 ) ) ;
#8262 = CARTESIAN_POINT ( 'NONE',  ( 5.385316468749999252, -29.96354166632527338, -3.109213912904138954 ) ) ;
#8263 = PRESENTATION_STYLE_ASSIGNMENT (( #5414 ) ) ;
#8264 = CARTESIAN_POINT ( 'NONE',  ( 5.385316468750001029, -29.25520833299193058, 3.109213912904135846 ) ) ;
#8265 = CARTESIAN_POINT ( 'NONE',  ( 1.467888652719048226, -1.349340926099361182, -3.492485675378536047 ) ) ;
#8266 = ORIENTED_EDGE ( 'NONE', *, *, #3984, .T. ) ;
#8267 = FACE_OUTER_BOUND ( 'NONE', #3917, .T. ) ;
#8268 = CARTESIAN_POINT ( 'NONE',  ( -5.250000000000000000, -27.40625000068279604, -6.429395695523604153E-16 ) ) ;
#8269 = CARTESIAN_POINT ( 'NONE',  ( -5.385316468750001029, -28.63020833299193413, -3.109213912904136734 ) ) ;
#8270 = ORIENTED_EDGE ( 'NONE', *, *, #6799, .T. ) ;
#8271 = CARTESIAN_POINT ( 'NONE',  ( 5.385316468750001029, -27.97395833299193413, 3.109213912904134958 ) ) ;
#8272 = CARTESIAN_POINT ( 'NONE',  ( -3.492485675378566246, -3.050659073900638507, 1.467888652718973397 ) ) ;
#8273 = DIRECTION ( 'NONE',  ( 0.000000000000000000, 1.000000000000000000, 0.000000000000000000 ) ) ;
#8274 = EDGE_CURVE ( 'NONE', #2936, #1704, #6969, .T. ) ;
#8275 = CARTESIAN_POINT ( 'NONE',  ( -1.406733260263394625, -28.48883544963257464, -5.250000000000000000 ) ) ;
#8276 = CARTESIAN_POINT ( 'NONE',  ( 1.431606283892619347, -7.149340926099362115, 3.507514324621464397 ) ) ;
#8277 = CARTESIAN_POINT ( 'NONE',  ( 3.616337804771879580E-16, -29.79687500034140157, -5.905927827173866440 ) ) ;
#8278 = CARTESIAN_POINT ( 'NONE',  ( 0.000000000000000000, -9.999999999999998224, 0.000000000000000000 ) ) ;
#8279 = APPLICATION_PROTOCOL_DEFINITION ( 'draft international standard', 'automotive_design', 1998, #5448 ) ;
#8280 = CARTESIAN_POINT ( 'NONE',  ( -5.385316468749998364, -29.80729166632526628, 3.109213912904140287 ) ) ;
#8281 = CARTESIAN_POINT ( 'NONE',  ( 1.431606283892619125, -3.949340926099361049, 3.507514324621464397 ) ) ;
#8282 = CARTESIAN_POINT ( 'NONE',  ( 5.385316468750001029, -29.47395833299193413, 3.109213912904135846 ) ) ;
#8283 = EDGE_CURVE ( 'NONE', #2547, #3872, #441, .T. ) ;
#8284 = CARTESIAN_POINT ( 'NONE',  ( -1.431606283892693066, -3.250659073900639129, 3.507514324621434199 ) ) ;
#8285 = ORIENTED_EDGE ( 'NONE', *, *, #4485, .T. ) ;
#8286 = DIRECTION ( 'NONE',  ( 0.000000000000000000, 1.000000000000000000, 0.000000000000000000 ) ) ;
#8287 = DIRECTION ( 'NONE',  ( 0.000000000000000000, -1.000000000000000000, 0.000000000000000000 ) ) ;
#8288 = ADVANCED_FACE ( 'NONE', ( #1188 ), #5316, .T. ) ;
#8289 = CARTESIAN_POINT ( 'NONE',  ( 1.467888652718972731, -3.450659073900639306, 3.492485675378566246 ) ) ;
#8290 = ORIENTED_EDGE ( 'NONE', *, *, #7525, .F. ) ;
#8291 = SURFACE_STYLE_FILL_AREA ( #2670 ) ;
#8292 = CARTESIAN_POINT ( 'NONE',  ( -5.249999999999999112, -28.97916666666666430, 3.031088913245538308 ) ) ;
#8293 = ORIENTED_EDGE ( 'NONE', *, *, #6301, .T. ) ;
#8294 = CARTESIAN_POINT ( 'NONE',  ( 5.114683531250000748, -29.60937500034139802, 0.000000000000000000 ) ) ;
#8295 = CARTESIAN_POINT ( 'NONE',  ( -3.007514324621463508, -3.549340926099361582, 1.224499502706077658 ) ) ;
#8296 = LINE ( 'NONE', #9028, #6881 ) ;
#8297 = CARTESIAN_POINT ( 'NONE',  ( 3.616337804771879580E-16, -27.60937500034139802, -5.905927827173866440 ) ) ;
#8298 = AXIS2_PLACEMENT_3D ( 'NONE', #1015, #7249, #2983 ) ;
#8299 = CARTESIAN_POINT ( 'NONE',  ( -6.972266317189433020E-16, -29.24999999931720396, -5.250000000000000000 ) ) ;
#8300 = DIRECTION ( 'NONE',  ( 0.000000000000000000, 1.000000000000000000, 0.000000000000000000 ) ) ;
#8301 = DIRECTION ( 'NONE',  ( 0.000000000000000000, -1.000000000000000000, 0.000000000000000000 ) ) ;
#8302 = CARTESIAN_POINT ( 'NONE',  ( 2.557341765625000818, -28.63020833367473017, -4.429445870380400052 ) ) ;
#8303 =( BOUNDED_CURVE ( )  B_SPLINE_CURVE ( 2, ( #4070, #7649, #6908, #6204, #9035, #5409, #8350, #434, #3282 ),
 .UNSPECIFIED., .F., .F. ) 
 B_SPLINE_CURVE_WITH_KNOTS ( ( 3, 2, 2, 2, 3 ),
 ( 0.5208333333333332593, 0.5277777777777777901, 0.5416666666666666297, 0.5555555555555555802, 0.5625000000000000000 ),
 .UNSPECIFIED. ) 
 CURVE ( )  GEOMETRIC_REPRESENTATION_ITEM ( )  RATIONAL_B_SPLINE_CURVE ( ( 0.9330127018922192983, 0.9330127018922187432, 1.000000000000000000, 0.8660254037844387076, 1.000000000000000000, 0.8660254037844387076, 1.000000000000000000, 0.9330127018922194093, 0.9330127018922194093 ) ) 
 REPRESENTATION_ITEM ( '' )  );
#8304 = CARTESIAN_POINT ( 'NONE',  ( 0.000000000000000000, -9.000000000000001776, 0.000000000000000000 ) ) ;
#8305 = CARTESIAN_POINT ( 'NONE',  ( -2.692658234375000514, -29.15104166632526983, -4.663820869356205989 ) ) ;
#8306 = DIRECTION ( 'NONE',  ( 0.000000000000000000, 1.000000000000000000, 0.000000000000000000 ) ) ;
#8307 = CARTESIAN_POINT ( 'NONE',  ( 0.000000000000000000, -27.00000000000000000, 0.000000000000000000 ) ) ;
#8308 = CARTESIAN_POINT ( 'NONE',  ( -2.692658234375000514, -28.90104166632526983, -4.663820869356205989 ) ) ;
#8309 = CARTESIAN_POINT ( 'NONE',  ( 3.507514324621465285, -2.749340926099361315, -1.431606283892619125 ) ) ;
#8310 = CARTESIAN_POINT ( 'NONE',  ( 3.507514324621465285, -2.749340926099361315, -1.431606283892619125 ) ) ;
#8311 = ORIENTED_EDGE ( 'NONE', *, *, #4971, .T. ) ;
#8312 = AXIS2_PLACEMENT_3D ( 'NONE', #2515, #926, #4518 ) ;
#8313 = CARTESIAN_POINT ( 'NONE',  ( 1.406733260263394625, -29.22991455036742536, -5.250000000000000000 ) ) ;
#8314 = CARTESIAN_POINT ( 'NONE',  ( 2.624999999999996891, -28.07291666734946389, 4.546633369868304797 ) ) ;
#8315 = CARTESIAN_POINT ( 'NONE',  ( -3.807688866302469071E-16, -29.92187499965859843, -6.218427825808274356 ) ) ;
#8316 = ORIENTED_EDGE ( 'NONE', *, *, #5142, .T. ) ;
#8317 = CIRCLE ( 'NONE', #282, 3.048902179152658931 ) ;
#8318 = CARTESIAN_POINT ( 'NONE',  ( 2.692658234374998738, -28.41145833299193413, -4.663820869356206877 ) ) ;
#8319 = CARTESIAN_POINT ( 'NONE',  ( 2.487701488670203354, -1.950659073900639084, 2.462045979635629323 ) ) ;
#8320 = PRODUCT_DEFINITION ( 'UNKNOWN', '', #1009, #3945 ) ;
#8321 = CARTESIAN_POINT ( 'NONE',  ( -1.000000000000000000, -35.00000000000000000, -1.118033988749894680 ) ) ;
#8322 = FACE_OUTER_BOUND ( 'NONE', #7970, .T. ) ;
#8323 = CIRCLE ( 'NONE', #2685, 2.999999999999999556 ) ;
#8324 = CARTESIAN_POINT ( 'NONE',  ( -1.975475456537005874E-15, -28.09375000068279604, 5.250000000000000000 ) ) ;
#8325 = CARTESIAN_POINT ( 'NONE',  ( -5.114683531250000748, -29.73437500034139802, -6.263680815196995234E-16 ) ) ;
#8326 = DIRECTION ( 'NONE',  ( 0.000000000000000000, 0.000000000000000000, 1.000000000000000000 ) ) ;
#8327 = AXIS2_PLACEMENT_3D ( 'NONE', #2612, #1909, #4734 ) ;
#8328 = APPLICATION_PROTOCOL_DEFINITION ( 'draft international standard', 'automotive_design', 1998, #5531 ) ;
#8329 = CARTESIAN_POINT ( 'NONE',  ( 5.385316468749999252, -28.93229166632526628, -3.109213912904139399 ) ) ;
#8330 = CARTESIAN_POINT ( 'NONE',  ( -3.492485675378536047, -8.149340926099361226, -1.467888652719048670 ) ) ;
#8331 = CARTESIAN_POINT ( 'NONE',  ( -1.406733260263384411, -29.55133545031537423, -5.250000000000006217 ) ) ;
#8332 = CARTESIAN_POINT ( 'NONE',  ( 2.692658234374998738, -29.41145833299193413, -4.663820869356206877 ) ) ;
#8333 = EDGE_CURVE ( 'NONE', #7933, #3248, #2346, .T. ) ;
#8334 = CARTESIAN_POINT ( 'NONE',  ( 3.500000000000000000, -3.750659073900639129, -0.01814118441313969030 ) ) ;
#8335 = DIRECTION ( 'NONE',  ( 0.000000000000000000, -0.000000000000000000, -1.000000000000000000 ) ) ;
#8336 = VECTOR ( 'NONE', #6894, 1000.000000000000114 ) ;
#8337 = CARTESIAN_POINT ( 'NONE',  ( 0.000000000000000000, -30.00000000000000000, 0.000000000000000000 ) ) ;
#8338 = EDGE_CURVE ( 'NONE', #116, #3013, #1235, .T. ) ;
#8339 = ORIENTED_EDGE ( 'NONE', *, *, #4027, .T. ) ;
#8340 = SHAPE_REPRESENTATION_RELATIONSHIP ( 'NONE' , 'NONE' ,  #6994, #3635 ) ;
#8341 = CARTESIAN_POINT ( 'NONE',  ( -5.250000000000000000, -28.50000000000000000, 0.000000000000000000 ) ) ;
#8342 = AXIS2_PLACEMENT_3D ( 'NONE', #2010, #3363, #6847 ) ;
#8343 = EDGE_CURVE ( 'NONE', #3606, #1434, #1191, .T. ) ;
#8344 = CARTESIAN_POINT ( 'NONE',  ( 2.557341765625000818, -28.06770833367473017, -4.429445870380400052 ) ) ;
#8345 = CARTESIAN_POINT ( 'NONE',  ( 0.01814118441320878086, -1.449340926099361493, -3.000000000000000444 ) ) ;
#8346 = CARTESIAN_POINT ( 'NONE',  ( 5.249999999999999112, -28.10416666666666785, -3.031088913245536975 ) ) ;
#8347 = CARTESIAN_POINT ( 'NONE',  ( 5.114683531249999859, -27.90104166700806587, -2.952963913586932776 ) ) ;
#8348 = DIRECTION ( 'NONE',  ( 0.000000000000000000, 0.000000000000000000, -1.000000000000000000 ) ) ;
#8349 = CARTESIAN_POINT ( 'NONE',  ( -5.114683531250000748, -28.79687500034139802, -6.263680815196995234E-16 ) ) ;
#8350 = CARTESIAN_POINT ( 'NONE',  ( -2.625000000000002220, -28.33333333333333215, 4.546633369868302132 ) ) ;
#8351 = CARTESIAN_POINT ( 'NONE',  ( -1.084901341431563923E-15, -29.23437500034139802, 5.905927827173866440 ) ) ;
#8352 = CARTESIAN_POINT ( 'NONE',  ( -5.249999999999999112, -28.77083333333333215, -3.031088913245534755 ) ) ;
#8353 = CARTESIAN_POINT ( 'NONE',  ( 2.624999999999998668, -28.77083333265053611, -4.546633369868303021 ) ) ;
#8354 = CARTESIAN_POINT ( 'NONE',  ( 2.692658234375002735, -30.02604166632526983, 4.663820869356205101 ) ) ;
#8355 = CARTESIAN_POINT ( 'NONE',  ( 5.249999999999999112, -29.51041666734945679, -3.031088913245534755 ) ) ;
#8356 = CARTESIAN_POINT ( 'NONE',  ( 1.142306659890740623E-15, -29.79687499965859843, 6.218427825808274356 ) ) ;
#8357 = CARTESIAN_POINT ( 'NONE',  ( 2.462045979635577364, -2.449340926099361049, 2.487701488670255312 ) ) ;
#8358 = CARTESIAN_POINT ( 'NONE',  ( -3.992485675378532939, -4.949340926099361937, -1.674995433905601683 ) ) ;
#8359 = ORIENTED_EDGE ( 'NONE', *, *, #8959, .T. ) ;
#8360 = FACE_OUTER_BOUND ( 'NONE', #5787, .T. ) ;
#8361 = CARTESIAN_POINT ( 'NONE',  ( -2.625000000000002220, -27.11458333401612819, 4.546633369868302132 ) ) ;
#8362 = ADVANCED_FACE ( 'NONE', ( #6166 ), #2682, .T. ) ;
#8363 =( BOUNDED_CURVE ( )  B_SPLINE_CURVE ( 2, ( #2640, #6116, #5511, #4720, #3335, #6865, #8944, #392, #4630 ),
 .UNSPECIFIED., .F., .T. ) 
 B_SPLINE_CURVE_WITH_KNOTS ( ( 3, 2, 2, 2, 3 ),
 ( 0.1875000000000000000, 0.1944444444444444475, 0.2083333333333333426, 0.2222222222222222099, 0.2291666666666666574 ),
 .UNSPECIFIED. ) 
 CURVE ( )  GEOMETRIC_REPRESENTATION_ITEM ( )  RATIONAL_B_SPLINE_CURVE ( ( 0.9330127018922194093, 0.9330127018922194093, 1.000000000000000000, 0.8660254037844387076, 1.000000000000000000, 0.8660254037844387076, 1.000000000000000000, 0.9330127018922194093, 0.9330127018922194093 ) ) 
 REPRESENTATION_ITEM ( '' )  );
#8364 = CARTESIAN_POINT ( 'NONE',  ( 2.692658234375002735, -29.52604166632526983, 4.663820869356205101 ) ) ;
#8365 = EDGE_CURVE ( 'NONE', #7146, #845, #4608, .T. ) ;
#8366 = ORIENTED_EDGE ( 'NONE', *, *, #6600, .T. ) ;
#8367 = CARTESIAN_POINT ( 'NONE',  ( 0.000000000000000000, -27.00000000000000000, 0.000000000000000000 ) ) ;
#8368 = CARTESIAN_POINT ( 'NONE',  ( 3.507514324621434199, -3.650659073900639928, 1.431606283892693066 ) ) ;
#8369 = CARTESIAN_POINT ( 'NONE',  ( 9.180150650966086169E-15, -28.59375000068279959, 5.249999999999999112 ) ) ;
#8370 = CARTESIAN_POINT ( 'NONE',  ( -1.406733260263397289, -28.38616454900183328, 5.249999999999997335 ) ) ;
#8371 = EDGE_CURVE ( 'NONE', #7471, #1378, #4721, .T. ) ;
#8372 = CARTESIAN_POINT ( 'NONE',  ( 5.250000000000000000, -28.03125000068279604, 0.000000000000000000 ) ) ;
#8373 = VECTOR ( 'NONE', #4711, 1000.000000000000000 ) ;
#8374 = CARTESIAN_POINT ( 'NONE',  ( -1.084901341431563923E-15, -28.17187500034139447, 5.905927827173866440 ) ) ;
#8375 = CARTESIAN_POINT ( 'NONE',  ( -5.249999999999997335, -28.16666666598386826, 3.031088913245538308 ) ) ;
#8376 = CARTESIAN_POINT ( 'NONE',  ( 1.142306659890740623E-15, -29.76562499965859843, 6.218427825808274356 ) ) ;
#8377 = CARTESIAN_POINT ( 'NONE',  ( 3.507514324621465285, -7.549340926099362470, -1.431606283892619125 ) ) ;
#8378 = CARTESIAN_POINT ( 'NONE',  ( -5.385316468750000141, -30.07812499965859843, 0.000000000000000000 ) ) ;
#8379 = CARTESIAN_POINT ( 'NONE',  ( -1.674995433905516196, -5.850659073900638774, -3.992485675378566690 ) ) ;
#8380 = VECTOR ( 'NONE', #4338, 1000.000000000000000 ) ;
#8381 = FACE_BOUND ( 'NONE', #2787, .T. ) ;
#8382 = LINE ( 'NONE', #6792, #3148 ) ;
#8383 =( BOUNDED_CURVE ( )  B_SPLINE_CURVE ( 2, ( #8689, #2978, #3719, #8087, #3074, #869, #2320, #8641, #8827 ),
 .UNSPECIFIED., .F., .F. ) 
 B_SPLINE_CURVE_WITH_KNOTS ( ( 3, 2, 2, 2, 3 ),
 ( 0.1875000000000000000, 0.1944444444444444475, 0.2083333333333333426, 0.2222222222222222099, 0.2291666666666666574 ),
 .UNSPECIFIED. ) 
 CURVE ( )  GEOMETRIC_REPRESENTATION_ITEM ( )  RATIONAL_B_SPLINE_CURVE ( ( 0.9330127018922194093, 0.9330127018922194093, 1.000000000000000000, 0.8660254037844387076, 1.000000000000000000, 0.8660254037844387076, 1.000000000000000000, 0.9330127018922194093, 0.9330127018922194093 ) ) 
 REPRESENTATION_ITEM ( '' )  );
#8384 = AXIS2_PLACEMENT_3D ( 'NONE', #5816, #1537, #4380 ) ;
#8385 = VERTEX_POINT ( 'NONE', #1850 ) ;
#8386 = CARTESIAN_POINT ( 'NONE',  ( -5.250000000000000000, -28.02083333333333215, -3.031088913245534755 ) ) ;
#8387 = CARTESIAN_POINT ( 'NONE',  ( 2.557341765624996821, -27.65104166700806587, 4.429445870380401828 ) ) ;
#8388 = CARTESIAN_POINT ( 'NONE',  ( -2.134148098076932953, -1.150659073900639040, -2.108492589042352705 ) ) ;
#8389 = CARTESIAN_POINT ( 'NONE',  ( 5.114683531249998971, -26.94270833367472662, 2.952963913586936329 ) ) ;
#8390 = CARTESIAN_POINT ( 'NONE',  ( -1.406733260263402174, -29.94866454968462577, 5.249999999999995559 ) ) ;
#8391 = EDGE_CURVE ( 'NONE', #2870, #7180, #9056, .T. ) ;
#8392 = CARTESIAN_POINT ( 'NONE',  ( 5.114683531250000748, -29.15104166700806232, -2.952963913586932776 ) ) ;
#8393 = PRODUCT ( 'barrel', 'barrel', '', ( #4785 ) ) ;
#8394 = FILL_AREA_STYLE_COLOUR ( '', #3279 ) ;
#8395 = CARTESIAN_POINT ( 'NONE',  ( 3.616337804771879580E-16, -29.10937500034139447, -5.905927827173866440 ) ) ;
#8396 = CARTESIAN_POINT ( 'NONE',  ( -1.406733260263402174, -29.19866454968462577, 5.249999999999995559 ) ) ;
#8397 = CARTESIAN_POINT ( 'NONE',  ( 5.250000000000000000, -29.29166666598386826, -3.031088913245536531 ) ) ;
#8398 = CARTESIAN_POINT ( 'NONE',  ( -5.385316468749998364, -30.08854166632526983, 3.109213912904140287 ) ) ;
#8399 = FILL_AREA_STYLE_COLOUR ( '', #1941 ) ;
#8400 = CARTESIAN_POINT ( 'NONE',  ( -0.01814118441321365544, -3.849340926099361404, 3.500000000000000000 ) ) ;
#8401 = CARTESIAN_POINT ( 'NONE',  ( -3.992485675378532939, -8.149340926099366555, -1.674995433905601683 ) ) ;
#8402 = EDGE_CURVE ( 'NONE', #977, #8760, #5031, .T. ) ;
#8403 = ORIENTED_EDGE ( 'NONE', *, *, #2854, .F. ) ;
#8404 = CARTESIAN_POINT ( 'NONE',  ( 0.000000000000000000, 1.000000000000000000, 0.000000000000000000 ) ) ;
#8405 = CARTESIAN_POINT ( 'NONE',  ( -5.114683531249999859, -29.50520833367473017, -2.952963913586935440 ) ) ;
#8406 = CARTESIAN_POINT ( 'NONE',  ( 2.692658234375002735, -30.02604166632526983, 4.663820869356205101 ) ) ;
#8407 = ORIENTED_EDGE ( 'NONE', *, *, #6679, .F. ) ;
#8408 = CARTESIAN_POINT ( 'NONE',  ( 2.692658234374998738, -29.16145833299193413, -4.663820869356206877 ) ) ;
#8409 = CARTESIAN_POINT ( 'NONE',  ( -1.431606283892693066, -6.450659073900639306, 3.507514324621434199 ) ) ;
#8410 = EDGE_CURVE ( 'NONE', #1704, #5007, #3337, .T. ) ;
#8411 = CARTESIAN_POINT ( 'NONE',  ( 0.000000000000000000, 81.00000000000001421, 0.000000000000000000 ) ) ;
#8412 = CARTESIAN_POINT ( 'NONE',  ( -5.385316468750000141, -30.07812499965859843, 0.000000000000000000 ) ) ;
#8413 = CARTESIAN_POINT ( 'NONE',  ( 1.000000000000000000, -29.00000000000000355, -2.431755684948965435 ) ) ;
#8414 = CARTESIAN_POINT ( 'NONE',  ( -2.462045979635576920, -8.049340926099361582, -2.487701488670255756 ) ) ;
#8415 = CARTESIAN_POINT ( 'NONE',  ( -2.557341765624999042, -28.02604166700806587, -4.429445870380400052 ) ) ;
#8416 = CYLINDRICAL_SURFACE ( 'NONE', #1839, 5.250000000000000000 ) ;
#8417 = DIRECTION ( 'NONE',  ( 0.000000000000000000, 0.000000000000000000, -1.000000000000000000 ) ) ;
#8418 = CARTESIAN_POINT ( 'NONE',  ( 2.487701488670255756, -6.049340926099361582, -2.462045979635577364 ) ) ;
#8419 = DIRECTION ( 'NONE',  ( 0.000000000000000000, 1.000000000000000000, 0.000000000000000000 ) ) ;
#8420 = CARTESIAN_POINT ( 'NONE',  ( -2.692658234375000514, -29.11979166632526983, -4.663820869356205989 ) ) ;
#8421 = CARTESIAN_POINT ( 'NONE',  ( -4.000000000000000000, 0.2493409260993615095, 0.01814118441313491634 ) ) ;
#8422 = PLANE ( 'NONE',  #6287 ) ;
#8423 = CARTESIAN_POINT ( 'NONE',  ( -3.117734906886650226, -2.800711225422160581E-13, 1.098956357287211194 ) ) ;
#8424 = EDGE_CURVE ( 'NONE', #3205, #2164, #7723, .T. ) ;
#8425 = EDGE_LOOP ( 'NONE', ( #1330, #2574 ) ) ;
#8426 =( NAMED_UNIT ( * ) SI_UNIT ( $, .STERADIAN. ) SOLID_ANGLE_UNIT ( ) );
#8427 = CARTESIAN_POINT ( 'NONE',  ( -2.624999999999996891, -29.95833333333333215, 4.546633369868304797 ) ) ;
#8428 = CARTESIAN_POINT ( 'NONE',  ( -5.114683531250001636, -27.21354166700806587, 2.952963913586931444 ) ) ;
#8429 = CARTESIAN_POINT ( 'NONE',  ( -2.134148098076932953, -2.750659073900639573, -2.108492589042352705 ) ) ;
#8430 = CARTESIAN_POINT ( 'NONE',  ( 2.557341765625000818, -27.88020833367473017, -4.429445870380400052 ) ) ;
#8431 = CARTESIAN_POINT ( 'NONE',  ( 0.000000000000000000, -30.00000000000000000, 0.000000000000000000 ) ) ;
#8432 =( BOUNDED_CURVE ( )  B_SPLINE_CURVE ( 2, ( #5124, #2957, #2344, #6521, #2204, #1552, #6472, #3695, #4487 ),
 .UNSPECIFIED., .F., .T. ) 
 B_SPLINE_CURVE_WITH_KNOTS ( ( 3, 2, 2, 2, 3 ),
 ( 0.6458333333333333703, 0.6527777777777777901, 0.6666666666666666297, 0.6805555555555555802, 0.6875000000000000000 ),
 .UNSPECIFIED. ) 
 CURVE ( )  GEOMETRIC_REPRESENTATION_ITEM ( )  RATIONAL_B_SPLINE_CURVE ( ( 0.9330127018922192983, 0.9330127018922198534, 1.000000000000000000, 0.8660254037844387076, 1.000000000000000000, 0.8660254037844387076, 1.000000000000000000, 0.9330127018922194093, 0.9330127018922194093 ) ) 
 REPRESENTATION_ITEM ( '' )  );
#8433 = CARTESIAN_POINT ( 'NONE',  ( 5.114683531249998971, -29.69270833367473017, 2.952963913586936329 ) ) ;
#8434 = CARTESIAN_POINT ( 'NONE',  ( 0.000000000000000000, 73.00000000000001421, 0.000000000000000000 ) ) ;
#8435 = CARTESIAN_POINT ( 'NONE',  ( -1.084901341431563923E-15, -28.98437500034139447, 5.905927827173866440 ) ) ;
#8436 = CARTESIAN_POINT ( 'NONE',  ( -1.406733260263394847, -29.67633545031537423, -5.250000000000000000 ) ) ;
#8437 = CARTESIAN_POINT ( 'NONE',  ( -5.250000000000000000, -29.70833333265053611, -3.031088913245534755 ) ) ;
#8438 = CARTESIAN_POINT ( 'NONE',  ( 0.000000000000000000, -30.00000000000000000, 0.000000000000000000 ) ) ;
#8439 = SURFACE_SIDE_STYLE ('',( #7695 ) ) ;
#8440 = CARTESIAN_POINT ( 'NONE',  ( 0.000000000000000000, 73.00000000000001421, 0.000000000000000000 ) ) ;
#8441 = CARTESIAN_POINT ( 'NONE',  ( -3.992485675378532939, -8.149340926099366555, -1.674995433905601683 ) ) ;
#8442 = CARTESIAN_POINT ( 'NONE',  ( -3.507514324621464397, -6.749340926099361759, 1.431606283892619347 ) ) ;
#8443 = EDGE_CURVE ( 'NONE', #5384, #8882, #1143, .T. ) ;
#8444 = ORIENTED_EDGE ( 'NONE', *, *, #4023, .T. ) ;
#8445 = DIRECTION ( 'NONE',  ( -0.000000000000000000, 1.000000000000000000, -0.000000000000000000 ) ) ;
#8446 = CARTESIAN_POINT ( 'NONE',  ( 2.624999999999996891, -27.07291666734946389, 4.546633369868304797 ) ) ;
#8447 = EDGE_CURVE ( 'NONE', #5172, #3304, #3868, .T. ) ;
#8448 = ORIENTED_EDGE ( 'NONE', *, *, #5988, .T. ) ;
#8449 = CARTESIAN_POINT ( 'NONE',  ( -2.692658234375000514, -29.36979166632526983, -4.663820869356205989 ) ) ;
#8450 = CARTESIAN_POINT ( 'NONE',  ( -4.000000000000000000, -1.350659073900638552, 0.01814118441313491634 ) ) ;
#8451 = MANIFOLD_SOLID_BREP ( 'Cavity1', #1042 ) ;
#8452 = DIRECTION ( 'NONE',  ( 0.000000000000000000, -1.000000000000000000, 0.000000000000000000 ) ) ;
#8453 = AXIS2_PLACEMENT_3D ( 'NONE', #4141, #1162, #1819 ) ;
#8454 = EDGE_CURVE ( 'NONE', #5103, #3312, #5442, .T. ) ;
#8455 = VERTEX_POINT ( 'NONE', #7793 ) ;
#8456 = CARTESIAN_POINT ( 'NONE',  ( 0.000000000000000000, 0.000000000000000000, -3.999999999999999112 ) ) ;
#8457 = DIRECTION ( 'NONE',  ( -0.000000000000000000, -1.000000000000000000, -0.000000000000000000 ) ) ;
#8458 = PLANE ( 'NONE',  #3874 ) ;
#8459 = AXIS2_PLACEMENT_3D ( 'NONE', #7667, #7574, #2651 ) ;
#8460 = CARTESIAN_POINT ( 'NONE',  ( 5.114683531249999859, -28.08854166700806232, -2.952963913586932776 ) ) ;
#8461 = CARTESIAN_POINT ( 'NONE',  ( 0.000000000000000000, 1.000000000000000000, 0.000000000000000000 ) ) ;
#8462 = CARTESIAN_POINT ( 'NONE',  ( 5.249999999999999112, -29.01041666734946389, -3.031088913245534755 ) ) ;
#8463 = CARTESIAN_POINT ( 'NONE',  ( 0.01814118441320878086, -4.649340926099361226, -3.000000000000000444 ) ) ;
#8464 = PLANE ( 'NONE',  #4877 ) ;
#8465 = CARTESIAN_POINT ( 'NONE',  ( 5.385316468750001029, -27.25520833299193413, 3.109213912904135846 ) ) ;
#8466 = CARTESIAN_POINT ( 'NONE',  ( 4.000000000000000000, -3.750659073900638685, -0.01814118441313441674 ) ) ;
#8467 = VECTOR ( 'NONE', #5725, 1000.000000000000000 ) ;
#8468 = MANIFOLD_SOLID_BREP ( 'Extrude-Thin1', #1479 ) ;
#8469 = PLANE ( 'NONE',  #3738 ) ;
#8470 = CARTESIAN_POINT ( 'NONE',  ( 2.033577675846918216E-14, -26.84375000068279959, 5.250000000000000888 ) ) ;
#8471 = EDGE_CURVE ( 'NONE', #6523, #4194, #443, .T. ) ;
#8472 = VERTEX_POINT ( 'NONE', #2726 ) ;
#8473 = FILL_AREA_STYLE_COLOUR ( '', #7392 ) ;
#8474 = AXIS2_PLACEMENT_3D ( 'NONE', #5897, #2370, #3814 ) ;
#8475 = CARTESIAN_POINT ( 'NONE',  ( -3.807688866302469071E-16, -27.14062499965860198, -6.218427825808274356 ) ) ;
#8476 = CARTESIAN_POINT ( 'NONE',  ( -2.557341765624999042, -27.52604166700806587, -4.429445870380400052 ) ) ;
#8477 = CARTESIAN_POINT ( 'NONE',  ( 3.000000000000000444, -0.5506590739006393953, -0.01814118441314496039 ) ) ;
#8478 = CIRCLE ( 'NONE', #600, 2.499999999999999556 ) ;
#8479 = CARTESIAN_POINT ( 'NONE',  ( 2.624999999999996891, -29.79166666666666430, 4.546633369868304797 ) ) ;
#8480 = CARTESIAN_POINT ( 'NONE',  ( 1.000000000000000000, -32.99989163573538775, 2.732192776429915426 ) ) ;
#8481 = CARTESIAN_POINT ( 'NONE',  ( 5.114683531250000748, -29.67187500034139802, 0.000000000000000000 ) ) ;
#8482 = MECHANICAL_DESIGN_GEOMETRIC_PRESENTATION_REPRESENTATION (  '', ( #3292 ), #4452 ) ;
#8483 = SURFACE_STYLE_FILL_AREA ( #2242 ) ;
#8484 = CARTESIAN_POINT ( 'NONE',  ( -1.084901341431563923E-15, -27.23437500034139802, 5.905927827173866440 ) ) ;
#8485 = CARTESIAN_POINT ( 'NONE',  ( -1.406733260263390628, -28.35491455036742181, 5.250000000000001776 ) ) ;
#8486 = CARTESIAN_POINT ( 'NONE',  ( 5.250000000000000000, -29.56249999931720041, -6.429395695523604153E-16 ) ) ;
#8487 = DIRECTION ( 'NONE',  ( 0.000000000000000000, -1.000000000000000000, 0.000000000000000000 ) ) ;
#8488 = CARTESIAN_POINT ( 'NONE',  ( -1.961808177976645418, 2.864554167741708363E-18, 2.934376452065968532 ) ) ;
#8489 = CARTESIAN_POINT ( 'NONE',  ( -1.975475456537005874E-15, -29.81249999999999645, 5.249999999999999112 ) ) ;
#8490 = CARTESIAN_POINT ( 'NONE',  ( 3.492485675378536047, -5.749340926099363536, 1.467888652719046672 ) ) ;
#8491 =( BOUNDED_CURVE ( )  B_SPLINE_CURVE ( 2, ( #2097, #6361, #1573, #4236, #2227, #3582, #7066, #2849, #8470 ),
 .UNSPECIFIED., .F., .T. ) 
 B_SPLINE_CURVE_WITH_KNOTS ( ( 3, 2, 2, 2, 3 ),
 ( 0.9375000000000000000, 0.9444444444444444198, 0.9583333333333333703, 0.9722222222222222099, 0.9791666666666667407 ),
 .UNSPECIFIED. ) 
 CURVE ( )  GEOMETRIC_REPRESENTATION_ITEM ( )  RATIONAL_B_SPLINE_CURVE ( ( 0.9330127018922194093, 0.9330127018922194093, 1.000000000000000000, 0.8660254037844387076, 1.000000000000000000, 0.8660254037844387076, 1.000000000000000000, 0.9330127018922187432, 0.9330127018922192983 ) ) 
 REPRESENTATION_ITEM ( '' )  );
#8492 = VERTEX_POINT ( 'NONE', #4206 ) ;
#8493 = VECTOR ( 'NONE', #6267, 1000.000000000000000 ) ;
#8494 = CARTESIAN_POINT ( 'NONE',  ( 0.000000000000000000, 75.00000000000000000, 0.000000000000000000 ) ) ;
#8495 = CARTESIAN_POINT ( 'NONE',  ( -5.114683531249999859, -29.75520833367473017, -2.952963913586935440 ) ) ;
#8496 = ORIENTED_EDGE ( 'NONE', *, *, #8501, .T. ) ;
#8497 = DIRECTION ( 'NONE',  ( 0.000000000000000000, -1.000000000000000000, 0.000000000000000000 ) ) ;
#8498 = CARTESIAN_POINT ( 'NONE',  ( 4.000000000000000000, -0.5506590739006383961, -0.01814118441313441674 ) ) ;
#8499 = DIRECTION ( 'NONE',  ( 0.000000000000000000, -1.000000000000000000, 0.000000000000000000 ) ) ;
#8500 = EDGE_LOOP ( 'NONE', ( #7544, #4750 ) ) ;
#8501 = EDGE_CURVE ( 'NONE', #183, #8537, #8851, .T. ) ;
#8502 = DIRECTION ( 'NONE',  ( 0.000000000000000000, 0.000000000000000000, 1.000000000000000000 ) ) ;
#8503 = DIRECTION ( 'NONE',  ( -0.000000000000000000, -1.000000000000000000, -0.000000000000000000 ) ) ;
#8504 = CARTESIAN_POINT ( 'NONE',  ( 0.000000000000000000, -30.00000000000000000, 0.000000000000000000 ) ) ;
#8505 = CARTESIAN_POINT ( 'NONE',  ( -5.114683531249999859, -29.25520833367473017, -2.952963913586935440 ) ) ;
#8506 = CARTESIAN_POINT ( 'NONE',  ( 3.122849337825750419E-16, -47.00000000000000000, -2.549999999999999822 ) ) ;
#8507 = CARTESIAN_POINT ( 'NONE',  ( -5.249999999999997335, -28.66666666598387181, 3.031088913245538308 ) ) ;
#8508 = CARTESIAN_POINT ( 'NONE',  ( 3.000000000000000444, -2.649340926099361671, 0.01814118441320859698 ) ) ;
#8509 = FACE_OUTER_BOUND ( 'NONE', #3651, .T. ) ;
#8510 = CARTESIAN_POINT ( 'NONE',  ( 5.385316468750001029, -28.25520833299193413, 3.109213912904135846 ) ) ;
#8511 = CARTESIAN_POINT ( 'NONE',  ( -1.638713065079245634, -0.05065907390063852794, 4.007514324621432422 ) ) ;
#8512 = CIRCLE ( 'NONE', #336, 4.250000000000000000 ) ;
#8513 = DIRECTION ( 'NONE',  ( 0.000000000000000000, 1.000000000000000000, 0.000000000000000000 ) ) ;
#8514 = CARTESIAN_POINT ( 'NONE',  ( 0.000000000000000000, -29.00000000000000355, 0.000000000000000000 ) ) ;
#8515 = ORIENTED_EDGE ( 'NONE', *, *, #6771, .T. ) ;
#8516 = CIRCLE ( 'NONE', #7175, 3.999999999999999112 ) ;
#8517 =( LENGTH_UNIT ( ) NAMED_UNIT ( * ) SI_UNIT ( .MILLI., .METRE. ) );
#8518 = CARTESIAN_POINT ( 'NONE',  ( 2.625000000000002220, -29.41666666666666785, 4.546633369868302132 ) ) ;
#8519 = CARTESIAN_POINT ( 'NONE',  ( 2.557341765625000818, -28.31770833367473017, -4.429445870380400052 ) ) ;
#8520 = CARTESIAN_POINT ( 'NONE',  ( -1.224499502706140497, -0.05065907390063940224, 3.007514324621436863 ) ) ;
#8521 = CARTESIAN_POINT ( 'NONE',  ( -2.624999999999998668, -29.66666666666666430, -4.546633369868303021 ) ) ;
#8522 = CARTESIAN_POINT ( 'NONE',  ( 5.250000000000000888, -29.39583333333332860, 3.031088913245533423 ) ) ;
#8523 = EDGE_CURVE ( 'NONE', #6529, #8492, #6077, .T. ) ;
#8524 = CARTESIAN_POINT ( 'NONE',  ( -1.084901341431563726E-15, -29.23437500034139802, 5.905927827173866440 ) ) ;
#8525 = CARTESIAN_POINT ( 'NONE',  ( -2.557341765624999042, -28.33854166700806587, -4.429445870380400052 ) ) ;
#8526 = CARTESIAN_POINT ( 'NONE',  ( -2.625000000000000444, -29.22916666598386826, -4.546633369868303021 ) ) ;
#8527 = CARTESIAN_POINT ( 'NONE',  ( 0.000000000000000000, 70.00000000000000000, 0.000000000000000000 ) ) ;
#8528 = CARTESIAN_POINT ( 'NONE',  ( -2.927826432601521311, -2.017599804162953374E-16, 2.262476218830554053 ) ) ;
#8529 = DIRECTION ( 'NONE',  ( 0.000000000000000000, 1.000000000000000000, 0.000000000000000000 ) ) ;
#8530 = CARTESIAN_POINT ( 'NONE',  ( -3.500000000000000000, -8.249340926099360871, -0.01814118441321344033 ) ) ;
#8531 = CARTESIAN_POINT ( 'NONE',  ( 3.500000000000000000, -7.449340926099361937, 0.01814118441321387054 ) ) ;
#8532 = ORIENTED_EDGE ( 'NONE', *, *, #8729, .T. ) ;
#8533 = CARTESIAN_POINT ( 'NONE',  ( -5.249999999999999112, -28.95833333265053611, -3.031088913245534755 ) ) ;
#8534 = CARTESIAN_POINT ( 'NONE',  ( 5.114683531250000748, -29.85937500034139802, 0.000000000000000000 ) ) ;
#8535 = ORIENTED_EDGE ( 'NONE', *, *, #8913, .T. ) ;
#8536 = EDGE_CURVE ( 'NONE', #3111, #813, #6384, .T. ) ;
#8537 = VERTEX_POINT ( 'NONE', #4430 ) ;
#8538 = CARTESIAN_POINT ( 'NONE',  ( -2.692658234375000514, -29.61979166632526983, -4.663820869356205989 ) ) ;
#8539 = CARTESIAN_POINT ( 'NONE',  ( 3.507514324621434199, -5.250659073900640905, 1.431606283892693066 ) ) ;
#8540 = DIRECTION ( 'NONE',  ( -0.000000000000000000, -0.000000000000000000, 1.000000000000000000 ) ) ;
#8541 = ORIENTED_EDGE ( 'NONE', *, *, #7167, .T. ) ;
#8542 = LINE ( 'NONE', #595, #1492 ) ;
#8543 = CARTESIAN_POINT ( 'NONE',  ( 6.429395695523604153E-16, 75.00000000000000000, -5.250000000000000000 ) ) ;
#8544 = CARTESIAN_POINT ( 'NONE',  ( 6.972266317189433020E-16, -27.93749999999999289, -5.249999999999999112 ) ) ;
#8545 = CARTESIAN_POINT ( 'NONE',  ( -5.114683531249999859, -28.50520833367473017, -2.952963913586935440 ) ) ;
#8546 = CARTESIAN_POINT ( 'NONE',  ( -1.467888652719046449, -2.149340926099360782, 3.492485675378536047 ) ) ;
#8547 = CARTESIAN_POINT ( 'NONE',  ( -5.250000000000000888, -28.88541666734946389, 3.031088913245533423 ) ) ;
#8548 = CARTESIAN_POINT ( 'NONE',  ( 3.000000000000000444, -4.249340926099360871, 0.01814118441320859698 ) ) ;
#8549 = CARTESIAN_POINT ( 'NONE',  ( -2.624999999999998668, -28.19791666734946389, -4.546633369868303021 ) ) ;
#8550 = CARTESIAN_POINT ( 'NONE',  ( -2.692658234374996518, -28.06770833299193413, 4.663820869356208654 ) ) ;
#8551 = CARTESIAN_POINT ( 'NONE',  ( -3.992485675378568022, -4.650659073900640372, 1.674995433905515529 ) ) ;
#8552 =( NAMED_UNIT ( * ) PLANE_ANGLE_UNIT ( ) SI_UNIT ( $, .RADIAN. ) );
#8553 = CARTESIAN_POINT ( 'NONE',  ( -2.624999999999998668, -27.69791666734946389, -4.546633369868303021 ) ) ;
#8554 = EDGE_LOOP ( 'NONE', ( #1019, #423, #4638, #7299 ) ) ;
#8555 = PRESENTATION_STYLE_ASSIGNMENT (( #5712 ) ) ;
#8556 = CARTESIAN_POINT ( 'NONE',  ( -2.625000000000000444, -29.79166666666666785, -4.546633369868303021 ) ) ;
#8557 = EDGE_LOOP ( 'NONE', ( #9024, #4444, #7841, #7598 ) ) ;
#8558 = FACE_OUTER_BOUND ( 'NONE', #4522, .T. ) ;
#8559 = CARTESIAN_POINT ( 'NONE',  ( -3.000000000000000444, -1.350659073900639440, 0.01814118441314532468 ) ) ;
#8560 = ORIENTED_EDGE ( 'NONE', *, *, #2475, .F. ) ;
#8561 = CARTESIAN_POINT ( 'NONE',  ( -2.624999999999998668, -29.41666666666666785, -4.546633369868303021 ) ) ;
#8562 = FACE_OUTER_BOUND ( 'NONE', #1783, .T. ) ;
#8563 = ADVANCED_FACE ( 'NONE', ( #8569, #150 ), #8010, .F. ) ;
#8564 = CARTESIAN_POINT ( 'NONE',  ( -2.557341765625002594, -27.50520833367473017, 4.429445870380399164 ) ) ;
#8565 = FILL_AREA_STYLE_COLOUR ( '', #8865 ) ;
#8566 = CARTESIAN_POINT ( 'NONE',  ( -5.114683531250000748, -27.54687500034139802, -6.263680815196995234E-16 ) ) ;
#8567 = CYLINDRICAL_SURFACE ( 'NONE', #5828, 5.250000000000000000 ) ;
#8568 = DIRECTION ( 'NONE',  ( 0.000000000000000000, -1.000000000000000000, 0.000000000000000000 ) ) ;
#8569 = FACE_BOUND ( 'NONE', #400, .T. ) ;
#8570 = DIRECTION ( 'NONE',  ( 0.8660254037844402619, 0.4999999999999970579, -0.000000000000000000 ) ) ;
#8571 = CARTESIAN_POINT ( 'NONE',  ( -2.557341765625002594, -29.75520833367473017, 4.429445870380399164 ) ) ;
#8572 = MECHANICAL_DESIGN_GEOMETRIC_PRESENTATION_REPRESENTATION (  '', ( #5742 ), #3981 ) ;
#8573 =( NAMED_UNIT ( * ) PLANE_ANGLE_UNIT ( ) SI_UNIT ( $, .RADIAN. ) );
#8574 = EDGE_LOOP ( 'NONE', ( #1022, #5692, #5739, #4213 ) ) ;
#8575 = CARTESIAN_POINT ( 'NONE',  ( 0.000000000000000000, -53.00000000000000000, 2.549999999999999822 ) ) ;
#8576 = CARTESIAN_POINT ( 'NONE',  ( 5.249999999999999112, -27.01041666734946389, -3.031088913245534755 ) ) ;
#8577 = CARTESIAN_POINT ( 'NONE',  ( 5.114683531250000748, -28.10937500034139447, 0.000000000000000000 ) ) ;
#8578 = ORIENTED_EDGE ( 'NONE', *, *, #3331, .T. ) ;
#8579 = PRODUCT_DEFINITION_FORMATION_WITH_SPECIFIED_SOURCE ( 'ANY', '', #3523, .NOT_KNOWN. ) ;
#8580 = VERTEX_POINT ( 'NONE', #1590 ) ;
#8581 = CARTESIAN_POINT ( 'NONE',  ( 5.249999999999997335, -26.80208333401613174, 3.031088913245538308 ) ) ;
#8582 = CARTESIAN_POINT ( 'NONE',  ( -0.01814118441313417734, -0.9506590739006385293, -4.000000000000000000 ) ) ;
#8583 = CARTESIAN_POINT ( 'NONE',  ( -6.972266317189433020E-16, -27.74999999931720041, -5.249999999999999112 ) ) ;
#8584 = VERTEX_POINT ( 'NONE', #196 ) ;
#8585 = DIRECTION ( 'NONE',  ( 0.000000000000000000, 1.000000000000000000, 0.000000000000000000 ) ) ;
#8586 = CARTESIAN_POINT ( 'NONE',  ( 1.000000000000000000, -32.99988997691444581, -2.732192653641477786 ) ) ;
#8587 = CARTESIAN_POINT ( 'NONE',  ( -2.557341765625002594, -27.69270833367473017, 4.429445870380399164 ) ) ;
#8588 = CARTESIAN_POINT ( 'NONE',  ( 0.000000000000000000, -30.00000000000000000, -6.250000000000000000 ) ) ;
#8589 = AXIS2_PLACEMENT_3D ( 'NONE', #4114, #7693, #4160 ) ;
#8590 = CARTESIAN_POINT ( 'NONE',  ( -0.01814118441320841310, -2.249340926099360871, 3.000000000000000444 ) ) ;
#8591 =( BOUNDED_CURVE ( )  B_SPLINE_CURVE ( 2, ( #660, #6368, #2858, #5719, #7868, #8522, #2150, #7212, #7915 ),
 .UNSPECIFIED., .F., .F. ) 
 B_SPLINE_CURVE_WITH_KNOTS ( ( 3, 2, 2, 2, 3 ),
 ( 0.7708333333333333703, 0.7777777777777777901, 0.7916666666666666297, 0.8055555555555555802, 0.8125000000000000000 ),
 .UNSPECIFIED. ) 
 CURVE ( )  GEOMETRIC_REPRESENTATION_ITEM ( )  RATIONAL_B_SPLINE_CURVE ( ( 0.9330127018922192983, 0.9330127018922198534, 1.000000000000000000, 0.8660254037844387076, 1.000000000000000000, 0.8660254037844387076, 1.000000000000000000, 0.9330127018922194093, 0.9330127018922194093 ) ) 
 REPRESENTATION_ITEM ( '' )  );
#8592 = CARTESIAN_POINT ( 'NONE',  ( 5.249999999999999112, -28.60416666666666430, -3.031088913245536975 ) ) ;
#8593 = CARTESIAN_POINT ( 'NONE',  ( 2.692658234375002735, -28.27604166632526628, 4.663820869356205101 ) ) ;
#8594 = CARTESIAN_POINT ( 'NONE',  ( -4.000000000000000000, -6.150659073900637708, 0.01814118441313491634 ) ) ;
#8595 = CARTESIAN_POINT ( 'NONE',  ( 1.406733260263394625, -27.19866454968463287, -5.250000000000000000 ) ) ;
#8596 = VECTOR ( 'NONE', #7280, 1000.000000000000000 ) ;
#8597 = DIRECTION ( 'NONE',  ( 0.000000000000000000, 1.000000000000000000, 0.000000000000000000 ) ) ;
#8598 = ORIENTED_EDGE ( 'NONE', *, *, #7785, .F. ) ;
#8599 = CARTESIAN_POINT ( 'NONE',  ( 1.113604000661152470E-15, -29.18750000000000000, 6.062177826491070398 ) ) ;
#8600 = ADVANCED_FACE ( 'NONE', ( #3743 ), #5914, .F. ) ;
#8601 = ORIENTED_EDGE ( 'NONE', *, *, #6379, .T. ) ;
#8602 =( GEOMETRIC_REPRESENTATION_CONTEXT ( 3 ) GLOBAL_UNCERTAINTY_ASSIGNED_CONTEXT ( ( #1614 ) ) GLOBAL_UNIT_ASSIGNED_CONTEXT ( ( #8120, #7977, #2259 ) ) REPRESENTATION_CONTEXT ( 'NONE', 'WORKASPACE' ) );
#8603 = CARTESIAN_POINT ( 'NONE',  ( 1.224499502706142273, -4.050659073900639839, -3.007514324621435531 ) ) ;
#8604 = ORIENTED_EDGE ( 'NONE', *, *, #5430, .T. ) ;
#8605 = CARTESIAN_POINT ( 'NONE',  ( 5.249999999999999112, -28.52083333333333215, 3.031088913245538308 ) ) ;
#8606 = ADVANCED_FACE ( 'NONE', ( #6656 ), #4339, .T. ) ;
#8607 = EDGE_CURVE ( 'NONE', #2876, #154, #6832, .T. ) ;
#8608 = CARTESIAN_POINT ( 'NONE',  ( -5.114683531250000748, -27.31770833367473017, -2.952963913586935440 ) ) ;
#8609 = CIRCLE ( 'NONE', #1782, 3.000000000000000444 ) ;
#8610 = CARTESIAN_POINT ( 'NONE',  ( 3.616337804771879580E-16, -27.85937500034139802, -5.905927827173866440 ) ) ;
#8611 = CIRCLE ( 'NONE', #7282, 2.549999999999999822 ) ;
#8612 = DIRECTION ( 'NONE',  ( 0.000000000000000000, 1.000000000000000000, 0.000000000000000000 ) ) ;
#8613 = CARTESIAN_POINT ( 'NONE',  ( 3.492485675378536047, -5.749340926099363536, 1.467888652719046672 ) ) ;
#8614 = CARTESIAN_POINT ( 'NONE',  ( -1.406733260263402174, -29.88616454900183328, 5.249999999999995559 ) ) ;
#8615 = CARTESIAN_POINT ( 'NONE',  ( 2.449293598294706414E-16, -20.00000000000000000, 2.000000000000000000 ) ) ;
#8616 = CARTESIAN_POINT ( 'NONE',  ( -2.557341765625002594, -29.50520833367473017, 4.429445870380399164 ) ) ;
#8617 = CARTESIAN_POINT ( 'NONE',  ( 3.500000000000000000, -4.249340926099360871, 0.01814118441321387054 ) ) ;
#8618 = ORIENTED_EDGE ( 'NONE', *, *, #5722, .F. ) ;
#8619 = CARTESIAN_POINT ( 'NONE',  ( -3.500000000000000000, -7.750659073900639129, 0.01814118441314011704 ) ) ;
#8620 = CARTESIAN_POINT ( 'NONE',  ( 2.033577675846918216E-14, -27.09375000068279604, 5.250000000000000888 ) ) ;
#8621 = CIRCLE ( 'NONE', #4616, 4.250000000000000000 ) ;
#8622 = CARTESIAN_POINT ( 'NONE',  ( -5.114683531249999859, -28.00520833367473017, -2.952963913586935440 ) ) ;
#8623 = EDGE_LOOP ( 'NONE', ( #1992, #3568, #2867, #5780 ) ) ;
#8624 = EDGE_LOOP ( 'NONE', ( #2742, #7615, #2098, #1128 ) ) ;
#8625 = CARTESIAN_POINT ( 'NONE',  ( -6.972266317189433020E-16, -29.81250000000000000, -5.250000000000000000 ) ) ;
#8626 = CARTESIAN_POINT ( 'NONE',  ( 2.692658234375002735, -27.77604166632526628, 4.663820869356205101 ) ) ;
#8627 = CARTESIAN_POINT ( 'NONE',  ( -4.007514324621467949, -0.3493409260993607379, 1.638713065079161924 ) ) ;
#8628 = CARTESIAN_POINT ( 'NONE',  ( -1.975475456537005874E-15, -27.56249999999999289, 5.250000000000000000 ) ) ;
#8629 = AXIS2_PLACEMENT_3D ( 'NONE', #909, #213, #2453 ) ;
#8630 = ORIENTED_EDGE ( 'NONE', *, *, #3665, .T. ) ;
#8631 = EDGE_CURVE ( 'NONE', #791, #4607, #8323, .T. ) ;
#8632 = CARTESIAN_POINT ( 'NONE',  ( -1.406733260263393293, -29.92633545031536713, -5.250000000000000000 ) ) ;
#8633 = CARTESIAN_POINT ( 'NONE',  ( -5.250000000000000000, -28.92708333401613174, -3.031088913245536531 ) ) ;
#8634 = CARTESIAN_POINT ( 'NONE',  ( 5.249999999999997335, -27.80208333401612819, 3.031088913245538308 ) ) ;
#8635 = CARTESIAN_POINT ( 'NONE',  ( 2.557341765625000818, -27.31770833367473017, -4.429445870380400052 ) ) ;
#8636 = CARTESIAN_POINT ( 'NONE',  ( 3.492485675378536047, -2.549340926099360694, 1.467888652719046672 ) ) ;
#8637 = CARTESIAN_POINT ( 'NONE',  ( -0.01814118441314477650, -0.9506590739006395285, -3.000000000000000444 ) ) ;
#8638 = DIRECTION ( 'NONE',  ( 1.000000000000000000, 0.000000000000000000, 0.000000000000000000 ) ) ;
#8639 = CARTESIAN_POINT ( 'NONE',  ( 3.992485675378568910, -7.050659073900638063, -1.674995433905514863 ) ) ;
#8640 = CARTESIAN_POINT ( 'NONE',  ( 1.113604000661152470E-15, -28.37499999931720396, 6.062177826491070398 ) ) ;
#8641 = CARTESIAN_POINT ( 'NONE',  ( 1.406733260263395735, -27.67633545031536713, 5.250000000000000000 ) ) ;
#8642 = DIRECTION ( 'NONE',  ( 0.000000000000000000, 0.000000000000000000, 1.000000000000000000 ) ) ;
#8643 =( BOUNDED_CURVE ( )  B_SPLINE_CURVE ( 2, ( #4203, #8436, #620, #7741, #1364, #4560, #5293, #273, #5341 ),
 .UNSPECIFIED., .F., .F. ) 
 B_SPLINE_CURVE_WITH_KNOTS ( ( 3, 2, 2, 2, 3 ),
 ( 0.1041666666666666713, 0.1111111111111111049, 0.1250000000000000000, 0.1388888888888888951, 0.1458333333333333426 ),
 .UNSPECIFIED. ) 
 CURVE ( )  GEOMETRIC_REPRESENTATION_ITEM ( )  RATIONAL_B_SPLINE_CURVE ( ( 0.9330127018922194093, 0.9330127018922194093, 1.000000000000000000, 0.8660254037844387076, 1.000000000000000000, 0.8660254037844387076, 1.000000000000000000, 0.9330127018922194093, 0.9330127018922194093 ) ) 
 REPRESENTATION_ITEM ( '' )  );
#8644 = CARTESIAN_POINT ( 'NONE',  ( 5.250000000000000000, -29.81249999931720041, -6.429395695523604153E-16 ) ) ;
#8645 = VERTEX_POINT ( 'NONE', #5771 ) ;
#8646 = DIRECTION ( 'NONE',  ( 1.000000000000000000, 0.000000000000000000, 0.000000000000000000 ) ) ;
#8647 = CARTESIAN_POINT ( 'NONE',  ( -2.692658234374996518, -28.78645833299193413, 4.663820869356208654 ) ) ;
#8648 = CARTESIAN_POINT ( 'NONE',  ( -5.250000000000000000, -28.75000000000000000, 0.000000000000000000 ) ) ;
#8649 = ORIENTED_EDGE ( 'NONE', *, *, #8402, .F. ) ;
#8650 = CARTESIAN_POINT ( 'NONE',  ( 5.385316468750000141, -27.70312499965860198, -6.595110575850215044E-16 ) ) ;
#8651 = CARTESIAN_POINT ( 'NONE',  ( 3.007514324621436863, -5.250659073900640017, 1.224499502706140719 ) ) ;
#8652 = ORIENTED_EDGE ( 'NONE', *, *, #4138, .T. ) ;
#8653 = CARTESIAN_POINT ( 'NONE',  ( -2.625000000000002220, -28.83333333333333215, 4.546633369868302132 ) ) ;
#8654 = CARTESIAN_POINT ( 'NONE',  ( 5.250000000000000000, -29.75000000000000000, 0.000000000000000000 ) ) ;
#8655 = CARTESIAN_POINT ( 'NONE',  ( -5.114683531250001636, -28.02604166700806587, 2.952963913586931444 ) ) ;
#8656 = VECTOR ( 'NONE', #2238, 1000.000000000000000 ) ;
#8657 =( LENGTH_UNIT ( ) NAMED_UNIT ( * ) SI_UNIT ( .MILLI., .METRE. ) );
#8658 = CARTESIAN_POINT ( 'NONE',  ( -2.557341765624999042, -27.33854166700806587, -4.429445870380400052 ) ) ;
#8659 = DIRECTION ( 'NONE',  ( 0.000000000000000000, 0.000000000000000000, 1.000000000000000000 ) ) ;
#8660 = CARTESIAN_POINT ( 'NONE',  ( 1.467888652719048226, -6.149340926099360338, -3.492485675378536047 ) ) ;
#8661 = EDGE_CURVE ( 'NONE', #3780, #5282, #6683, .T. ) ;
#8662 = CARTESIAN_POINT ( 'NONE',  ( -5.250000000000000000, -29.93749999931720041, 0.000000000000000000 ) ) ;
#8663 = AXIS2_PLACEMENT_3D ( 'NONE', #1451, #895, #2339 ) ;
#8664 = CARTESIAN_POINT ( 'NONE',  ( -2.624999999999998668, -29.69791666734946034, -4.546633369868303021 ) ) ;
#8665 = DIRECTION ( 'NONE',  ( 0.000000000000000000, -1.000000000000000000, 0.000000000000000000 ) ) ;
#8666 = ORIENTED_EDGE ( 'NONE', *, *, #3134, .T. ) ;
#8667 = CARTESIAN_POINT ( 'NONE',  ( 1.975475456537005874E-15, -27.18750000000000000, 5.250000000000000000 ) ) ;
#8668 = CARTESIAN_POINT ( 'NONE',  ( 1.406733260263394625, -26.97991455036742181, -5.250000000000000000 ) ) ;
#8669 = CARTESIAN_POINT ( 'NONE',  ( 5.114683531249999859, -28.58854166700806232, -2.952963913586932776 ) ) ;
#8670 = AXIS2_PLACEMENT_3D ( 'NONE', #2751, #3530, #8417 ) ;
#8671 = ORIENTED_EDGE ( 'NONE', *, *, #4211, .T. ) ;
#8672 = CARTESIAN_POINT ( 'NONE',  ( 1.406733260263403507, -29.57366454968462932, -5.249999999999994671 ) ) ;
#8673 = EDGE_CURVE ( 'NONE', #3243, #7319, #841, .T. ) ;
#8674 = CARTESIAN_POINT ( 'NONE',  ( 2.692658234374998738, -27.19270833299193413, -4.663820869356206877 ) ) ;
#8675 = CARTESIAN_POINT ( 'NONE',  ( -1.638713065079245634, -4.850659073900639662, 4.007514324621432422 ) ) ;
#8676 = ORIENTED_EDGE ( 'NONE', *, *, #1659, .T. ) ;
#8677 = ADVANCED_FACE ( 'NONE', ( #8756, #5069 ), #2293, .T. ) ;
#8678 = CARTESIAN_POINT ( 'NONE',  ( -3.500000000000000000, -7.750659073900639129, 0.01814118441314011704 ) ) ;
#8679 = CARTESIAN_POINT ( 'NONE',  ( -2.624999999999998668, -29.44791666734946034, -4.546633369868303021 ) ) ;
#8680 = CARTESIAN_POINT ( 'NONE',  ( 1.142306659890740623E-15, -28.29687499965860553, 6.218427825808274356 ) ) ;
#8681 = CARTESIAN_POINT ( 'NONE',  ( -5.114683531250000748, -27.46354166700806232, 2.952963913586931888 ) ) ;
#8682 = CARTESIAN_POINT ( 'NONE',  ( 0.01814118441321408565, -1.449340926099361271, -3.500000000000000000 ) ) ;
#8683 = CARTESIAN_POINT ( 'NONE',  ( 1.975475456537005874E-15, -28.87499999931720396, 5.250000000000000000 ) ) ;
#8684 = CARTESIAN_POINT ( 'NONE',  ( -2.992485675378564469, -3.050659073900639839, 1.260781871532430820 ) ) ;
#8685 = UNCERTAINTY_MEASURE_WITH_UNIT (LENGTH_MEASURE( 1.000000000000000082E-05 ), #1080, 'distance_accuracy_value', 'NONE');
#8686 = CARTESIAN_POINT ( 'NONE',  ( -5.249999999999997335, -27.41666666598387181, 3.031088913245538308 ) ) ;
#8687 = CARTESIAN_POINT ( 'NONE',  ( 1.674995433905601239, -2.949340926099360605, -3.992485675378532939 ) ) ;
#8688 = CARTESIAN_POINT ( 'NONE',  ( -2.625000000000000444, -27.97916666598386826, -4.546633369868303021 ) ) ;
#8689 = CARTESIAN_POINT ( 'NONE',  ( -6.972266317189433020E-16, -27.56249999999999645, -5.250000000000000000 ) ) ;
#8690 = CARTESIAN_POINT ( 'NONE',  ( -3.492485675378535603, -3.349340926099361404, -1.467888652719048670 ) ) ;
#8691 = CARTESIAN_POINT ( 'NONE',  ( 2.624999999999998668, -29.52083333265053611, -4.546633369868303021 ) ) ;
#8692 = ORIENTED_EDGE ( 'NONE', *, *, #652, .T. ) ;
#8693 = SURFACE_SIDE_STYLE ('',( #3772 ) ) ;
#8694 = CARTESIAN_POINT ( 'NONE',  ( -5.385316468750001029, -28.09895833299193413, -3.109213912904136734 ) ) ;
#8695 = CARTESIAN_POINT ( 'NONE',  ( -1.674995433905599462, -6.949340926099362825, 3.992485675378533383 ) ) ;
#8696 = CYLINDRICAL_SURFACE ( 'NONE', #4438, 5.250000000000000000 ) ;
#8697 = ORIENTED_EDGE ( 'NONE', *, *, #3278, .T. ) ;
#8698 = FACE_OUTER_BOUND ( 'NONE', #339, .T. ) ;
#8699 = CARTESIAN_POINT ( 'NONE',  ( -3.500000000000000000, 0.2493409260993610654, 0.01814118441314012051 ) ) ;
#8700 = EDGE_LOOP ( 'NONE', ( #3989, #4056, #6436, #8697 ) ) ;
#8701 = CARTESIAN_POINT ( 'NONE',  ( 5.250000000000000000, -27.47916666666666430, -3.031088913245534755 ) ) ;
#8702 = CARTESIAN_POINT ( 'NONE',  ( -2.557341765625002594, -28.00520833367473017, 4.429445870380399164 ) ) ;
#8703 = SHAPE_REPRESENTATION_RELATIONSHIP ( 'NONE' , 'NONE' ,  #4551, #4641 ) ;
#8704 = DIRECTION ( 'NONE',  ( 0.000000000000000000, 1.000000000000000000, 0.000000000000000000 ) ) ;
#8705 = CARTESIAN_POINT ( 'NONE',  ( -2.033577675846918216E-14, -28.93750000000000000, 5.250000000000000888 ) ) ;
#8706 = CARTESIAN_POINT ( 'NONE',  ( -0.01814118441321365544, -3.849340926099361404, 3.500000000000000000 ) ) ;
#8707 = CARTESIAN_POINT ( 'NONE',  ( 0.000000000000000000, -46.00000000000000000, 0.000000000000000000 ) ) ;
#8708 = CARTESIAN_POINT ( 'NONE',  ( -5.249999999999999112, -28.27083333333332860, -3.031088913245534755 ) ) ;
#8709 = CARTESIAN_POINT ( 'NONE',  ( 2.487701488670255756, -7.649340926099361226, -2.462045979635577364 ) ) ;
#8710 = CARTESIAN_POINT ( 'NONE',  ( 0.000000000000000000, -27.00000000000000000, 0.000000000000000000 ) ) ;
#8711 = VERTEX_POINT ( 'NONE', #3091 ) ;
#8712 = DIRECTION ( 'NONE',  ( 0.000000000000000000, 0.000000000000000000, 1.000000000000000000 ) ) ;
#8713 = CARTESIAN_POINT ( 'NONE',  ( 3.367778697655221012E-16, -28.00000000000000000, 2.750000000000000000 ) ) ;
#8714 = CARTESIAN_POINT ( 'NONE',  ( -5.114683531250000748, -28.73437500034139802, -6.263680815196995234E-16 ) ) ;
#8715 = ORIENTED_EDGE ( 'NONE', *, *, #4351, .F. ) ;
#8716 = CARTESIAN_POINT ( 'NONE',  ( -5.249999999999999112, -29.77083333333332860, -3.031088913245534755 ) ) ;
#8717 = CARTESIAN_POINT ( 'NONE',  ( -2.692658234374996518, -28.06770833299193413, 4.663820869356208654 ) ) ;
#8718 = CARTESIAN_POINT ( 'NONE',  ( -1.638713065079245634, -3.250659073900639129, 4.007514324621432422 ) ) ;
#8719 = EDGE_CURVE ( 'NONE', #7275, #803, #3830, .T. ) ;
#8720 = CARTESIAN_POINT ( 'NONE',  ( 0.000000000000000000, -20.00000000000000000, 0.000000000000000000 ) ) ;
#8721 = EDGE_LOOP ( 'NONE', ( #202, #163, #7368 ) ) ;
#8722 = EDGE_CURVE ( 'NONE', #1724, #6874, #7921, .T. ) ;
#8723 = CARTESIAN_POINT ( 'NONE',  ( -5.250000000000000888, -28.88541666734946745, 3.031088913245532979 ) ) ;
#8724 =( BOUNDED_CURVE ( )  B_SPLINE_CURVE ( 2, ( #6160, #338, #3192, #700, #1974, #4885, #5631, #4972, #3372, #1361, #4805, #8433, #8481, #9164, #5589, #532, #4112, #617, #7826, #1443, #5675, #5547, #7077, #7689, #9034, #3504, #6369, #9080, #7647, #4844, #2105, #7784, #3458, #8524, #6944, #4929, #6203, #8392, #4288, #9123, #1404, #6990, #2676, #4244, #1274, #3545, #7737, #1313, #661, #9, #5505, #4200, #6289, #2859, #8349, #573, #4154, #3418, #6327, #7036, #2151, #6248, #2721, #2019, #2769, #2059, #2811, #934, #746, #5817, #7309, #8006, #55, #4381, #6608, #189, #1681, #237, #7869, #1585, #7961, #4335, #3044, #7122, #2946, #2382, #6507, #1634, #5862, #94, #7213, #8655, #8702, #2333, #1491, #7168, #3683, #5063, #5211, #3086, #5163, #6415, #3592, #1540, #2903, #3736, #4426, #3783, #143, #4472, #5909, #8750, #7916, #5720, #2995, #8054, #8564, #2287, #2192, #5014, #795, #3639, #6462, #837, #5765, #8608, #2240, #5113, #7259, #887, #6559, #6147, #8928, #4656, #3966, #5348, #6697, #375, #3223, #2523, #3179, #1078, #1879, #2429, #325 ),
 .UNSPECIFIED., .F., .F. ) 
 B_SPLINE_CURVE_WITH_KNOTS ( ( 3, 2, 2, 2, 2, 2, 2, 2, 2, 2, 2, 2, 2, 2, 2, 2, 2, 2, 2, 2, 2, 2, 2, 2, 2, 2, 2, 2, 2, 2, 2, 2, 2, 2, 2, 2, 2, 2, 2, 2, 2, 2, 2, 2, 2, 2, 2, 2, 2, 2, 2, 2, 2, 2, 2, 2, 2, 2, 2, 2, 2, 2, 2, 2, 2, 2, 2, 2, 2, 2, 2, 2, 3 ),
 ( 0.000000000000000000, 0.01388888888888888812, 0.02777777777777777624, 0.04166666666666666435, 0.05555555555555555247, 0.06944444444444444753, 0.08333333333333332871, 0.09722222222222222376, 0.1111111111111111049, 0.1250000000000000000, 0.1388888888888888951, 0.1527777777777777901, 0.1666666666666666574, 0.1805555555555555525, 0.1944444444444444475, 0.2083333333333333426, 0.2222222222222222099, 0.2361111111111111049, 0.2500000000000000000, 0.2638888888888888951, 0.2777777777777777901, 0.2916666666666666852, 0.3055555555555555802, 0.3194444444444444198, 0.3333333333333333148, 0.3472222222222222099, 0.3611111111111111049, 0.3750000000000000000, 0.3888888888888888951, 0.4027777777777777901, 0.4166666666666666852, 0.4305555555555555802, 0.4444444444444444198, 0.4583333333333333148, 0.4722222222222222099, 0.4861111111111111049, 0.5000000000000000000, 0.5138888888888888395, 0.5277777777777777901, 0.5416666666666666297, 0.5555555555555555802, 0.5694444444444444198, 0.5833333333333333703, 0.5972222222222222099, 0.6111111111111111605, 0.6250000000000000000, 0.6388888888888888395, 0.6527777777777777901, 0.6666666666666666297, 0.6805555555555555802, 0.6944444444444444198, 0.7083333333333333703, 0.7222222222222222099, 0.7361111111111111605, 0.7500000000000000000, 0.7638888888888888395, 0.7777777777777777901, 0.7916666666666666297, 0.8055555555555555802, 0.8194444444444444198, 0.8333333333333333703, 0.8472222222222222099, 0.8611111111111111605, 0.8750000000000000000, 0.8888888888888888395, 0.9027777777777777901, 0.9166666666666666297, 0.9305555555555555802, 0.9444444444444444198, 0.9583333333333333703, 0.9722222222222222099, 0.9861111111111111605, 1.000000000000000000 ),
 .UNSPECIFIED. ) 
 CURVE ( )  GEOMETRIC_REPRESENTATION_ITEM ( )  RATIONAL_B_SPLINE_CURVE ( ( 1.000000000000000000, 0.8660254037844387076, 1.000000000000000000, 0.8660254037844387076, 1.000000000000000000, 0.8660254037844387076, 1.000000000000000000, 0.8660254037844387076, 1.000000000000000000, 0.8660254037844387076, 1.000000000000000000, 0.8660254037844387076, 1.000000000000000000, 0.8660254037844387076, 1.000000000000000000, 0.8660254037844387076, 1.000000000000000000, 0.8660254037844387076, 1.000000000000000000, 0.8660254037844387076, 1.000000000000000000, 0.8660254037844387076, 1.000000000000000000, 0.8660254037844387076, 1.000000000000000000, 0.8660254037844387076, 1.000000000000000000, 0.8660254037844387076, 1.000000000000000000, 0.8660254037844387076, 1.000000000000000000, 0.8660254037844387076, 1.000000000000000000, 0.8660254037844387076, 1.000000000000000000, 0.8660254037844387076, 1.000000000000000000, 0.8660254037844387076, 1.000000000000000000, 0.8660254037844387076, 1.000000000000000000, 0.8660254037844387076, 1.000000000000000000, 0.8660254037844387076, 1.000000000000000000, 0.8660254037844387076, 1.000000000000000000, 0.8660254037844387076, 1.000000000000000000, 0.8660254037844387076, 1.000000000000000000, 0.8660254037844387076, 1.000000000000000000, 0.8660254037844387076, 1.000000000000000000, 0.8660254037844387076, 1.000000000000000000, 0.8660254037844387076, 1.000000000000000000, 0.8660254037844387076, 1.000000000000000000, 0.8660254037844387076, 1.000000000000000000, 0.8660254037844387076, 1.000000000000000000, 0.8660254037844387076, 1.000000000000000000, 0.8660254037844387076, 1.000000000000000000, 0.8660254037844387076, 1.000000000000000000, 0.8660254037844387076, 1.000000000000000000, 0.8660254037844387076, 1.000000000000000000, 0.8660254037844387076, 1.000000000000000000, 0.8660254037844387076, 1.000000000000000000, 0.8660254037844387076, 1.000000000000000000, 0.8660254037844387076, 1.000000000000000000, 0.8660254037844387076, 1.000000000000000000, 0.8660254037844387076, 1.000000000000000000, 0.8660254037844387076, 1.000000000000000000, 0.8660254037844387076, 1.000000000000000000, 0.8660254037844387076, 1.000000000000000000, 0.8660254037844387076, 1.000000000000000000, 0.8660254037844387076, 1.000000000000000000, 0.8660254037844387076, 1.000000000000000000, 0.8660254037844387076, 1.000000000000000000, 0.8660254037844387076, 1.000000000000000000, 0.8660254037844387076, 1.000000000000000000, 0.8660254037844387076, 1.000000000000000000, 0.8660254037844387076, 1.000000000000000000, 0.8660254037844387076, 1.000000000000000000, 0.8660254037844387076, 1.000000000000000000, 0.8660254037844387076, 1.000000000000000000, 0.8660254037844387076, 1.000000000000000000, 0.8660254037844387076, 1.000000000000000000, 0.8660254037844387076, 1.000000000000000000, 0.8660254037844387076, 1.000000000000000000, 0.8660254037844387076, 1.000000000000000000, 0.8660254037844387076, 1.000000000000000000, 0.8660254037844387076, 1.000000000000000000, 0.8660254037844387076, 1.000000000000000000, 0.8660254037844387076, 1.000000000000000000, 0.8660254037844387076, 1.000000000000000000, 0.8660254037844387076, 1.000000000000000000, 0.8660254037844387076, 1.000000000000000000, 0.8660254037844387076, 1.000000000000000000, 0.8660254037844387076, 1.000000000000000000, 0.8660254037844387076, 1.000000000000000000 ) ) 
 REPRESENTATION_ITEM ( '' )  );
#8725 = CARTESIAN_POINT ( 'NONE',  ( 1.142306659890740623E-15, -27.79687499965860198, 6.218427825808274356 ) ) ;
#8726 = CARTESIAN_POINT ( 'NONE',  ( 2.557341765624996821, -26.90104166700806232, 4.429445870380401828 ) ) ;
#8727 = DIRECTION ( 'NONE',  ( 0.000000000000000000, -1.000000000000000000, 0.000000000000000000 ) ) ;
#8728 = CARTESIAN_POINT ( 'NONE',  ( 1.406733260263395735, -28.86383544963257464, 5.250000000000000000 ) ) ;
#8729 = EDGE_CURVE ( 'NONE', #3081, #1286, #4751, .T. ) ;
#8730 = CARTESIAN_POINT ( 'NONE',  ( 2.992485675378565357, -3.850659073900639662, -1.260781871532430376 ) ) ;
#8731 = CARTESIAN_POINT ( 'NONE',  ( 6.429395695523604153E-16, -9.000000000000001776, -5.250000000000000000 ) ) ;
#8732 = AXIS2_PLACEMENT_3D ( 'NONE', #270, #8140, #3123 ) ;
#8733 = CARTESIAN_POINT ( 'NONE',  ( 1.638713065079161924, -2.349340926099360960, 4.007514324621467949 ) ) ;
#8734 = CARTESIAN_POINT ( 'NONE',  ( 5.250000000000000000, -28.29166666598387181, -3.031088913245536531 ) ) ;
#8735 = CARTESIAN_POINT ( 'NONE',  ( -6.972266317189433020E-16, -27.74999999931720041, -5.250000000000000000 ) ) ;
#8736 = CARTESIAN_POINT ( 'NONE',  ( -2.462045979635576920, -4.849340926099361404, -2.487701488670255756 ) ) ;
#8737 = CARTESIAN_POINT ( 'NONE',  ( 2.625000000000002220, -29.10416666598386826, 4.546633369868302132 ) ) ;
#8738 = SHAPE_REPRESENTATION_RELATIONSHIP ( 'NONE' , 'NONE' ,  #2791, #2538 ) ;
#8739 = CARTESIAN_POINT ( 'NONE',  ( 1.142306659890740623E-15, -28.76562499965860553, 6.218427825808274356 ) ) ;
#8740 = CARTESIAN_POINT ( 'NONE',  ( 1.638713065079161924, -2.349340926099360960, 4.007514324621467949 ) ) ;
#8741 = CARTESIAN_POINT ( 'NONE',  ( -2.625000000000002220, -27.33333333333333215, 4.546633369868302132 ) ) ;
#8742 = EDGE_LOOP ( 'NONE', ( #3561, #7530, #6119, #8821 ) ) ;
#8743 = CARTESIAN_POINT ( 'NONE',  ( -3.807688866302469071E-16, -27.39062499965860198, -6.218427825808274356 ) ) ;
#8744 = CARTESIAN_POINT ( 'NONE',  ( -2.108492589042352261, -4.750659073900640017, 2.134148098076933397 ) ) ;
#8745 = VERTEX_POINT ( 'NONE', #1546 ) ;
#8746 = CARTESIAN_POINT ( 'NONE',  ( -5.250000000000000888, -28.35416666666666785, 3.031088913245532979 ) ) ;
#8747 = AXIS2_PLACEMENT_3D ( 'NONE', #3447, #4788, #3309 ) ;
#8748 = PRODUCT_DEFINITION_SHAPE ( 'NONE', 'NONE',  #9194 ) ;
#8749 = EDGE_CURVE ( 'NONE', #187, #1130, #1478, .T. ) ;
#8750 = CARTESIAN_POINT ( 'NONE',  ( 3.616337804771879580E-16, -27.60937500034139802, -5.905927827173866440 ) ) ;
#8751 = ADVANCED_FACE ( 'NONE', ( #6007 ), #8846, .F. ) ;
#8752 = VECTOR ( 'NONE', #7292, 1000.000000000000000 ) ;
#8753 = CARTESIAN_POINT ( 'NONE',  ( -5.250000000000000000, -27.52083333333333570, -3.031088913245534755 ) ) ;
#8754 = CARTESIAN_POINT ( 'NONE',  ( 2.557341765625000818, -29.81770833367473372, -4.429445870380400052 ) ) ;
#8755 = CARTESIAN_POINT ( 'NONE',  ( 1.467888652719048226, -4.549340926099360694, -3.492485675378536047 ) ) ;
#8756 = FACE_BOUND ( 'NONE', #3798, .T. ) ;
#8757 = CARTESIAN_POINT ( 'NONE',  ( -5.249999999999997335, -27.72916666666666430, 3.031088913245538308 ) ) ;
#8758 = CARTESIAN_POINT ( 'NONE',  ( 3.616337804771879580E-16, -29.35937500034139802, -5.905927827173866440 ) ) ;
#8759 = DIRECTION ( 'NONE',  ( 0.000000000000000000, 0.000000000000000000, 1.000000000000000000 ) ) ;
#8760 = VERTEX_POINT ( 'NONE', #6704 ) ;
#8761 = VECTOR ( 'NONE', #286, 1000.000000000000000 ) ;
#8762 = CARTESIAN_POINT ( 'NONE',  ( -6.972266317189433020E-16, -27.06250000000000000, -5.249999999999999112 ) ) ;
#8763 = CARTESIAN_POINT ( 'NONE',  ( 2.557341765624996821, -28.15104166700806587, 4.429445870380401828 ) ) ;
#8764 = ORIENTED_EDGE ( 'NONE', *, *, #3959, .T. ) ;
#8765 = CARTESIAN_POINT ( 'NONE',  ( 0.000000000000000000, -30.00000000000000000, 0.000000000000000000 ) ) ;
#8766 = CARTESIAN_POINT ( 'NONE',  ( -5.385316468750000141, -27.10937499965860198, 0.000000000000000000 ) ) ;
#8767 = CARTESIAN_POINT ( 'NONE',  ( -0.01814118441313417734, -2.550659073900638951, -4.000000000000000000 ) ) ;
#8768 = CARTESIAN_POINT ( 'NONE',  ( 2.624999999999998668, -29.27083333265053611, -4.546633369868303021 ) ) ;
#8769 = CARTESIAN_POINT ( 'NONE',  ( -5.385316468749998364, -27.58854166632526983, 3.109213912904140287 ) ) ;
#8770 = EDGE_LOOP ( 'NONE', ( #5808, #4400, #5470, #6024 ) ) ;
#8771 = VECTOR ( 'NONE', #9145, 1000.000000000000000 ) ;
#8772 = CARTESIAN_POINT ( 'NONE',  ( 1.406733260263393293, -29.82366454968462932, -5.250000000000000000 ) ) ;
#8773 = CARTESIAN_POINT ( 'NONE',  ( 3.712013335537174572E-16, -28.96875000068279959, -6.062177826491070398 ) ) ;
#8774 = CARTESIAN_POINT ( 'NONE',  ( -5.385316468750000141, -27.60937499965860198, 0.000000000000000000 ) ) ;
#8775 = CARTESIAN_POINT ( 'NONE',  ( 5.114683531250000748, -27.10937500034139802, 0.000000000000000000 ) ) ;
#8776 = ORIENTED_EDGE ( 'NONE', *, *, #2253, .F. ) ;
#8777 = CARTESIAN_POINT ( 'NONE',  ( 2.624999999999998668, -28.77083333265053611, -4.546633369868303021 ) ) ;
#8778 = CARTESIAN_POINT ( 'NONE',  ( -2.108492589042352261, -1.550659073900639395, 2.134148098076933397 ) ) ;
#8779 = CARTESIAN_POINT ( 'NONE',  ( -1.000000000000000000, -29.00000000000000355, -3.048902179152658931 ) ) ;
#8780 = ADVANCED_FACE ( 'NONE', ( #3927 ), #1834, .F. ) ;
#8781 =( BOUNDED_CURVE ( )  B_SPLINE_CURVE ( 2, ( #1292, #2653, #4781, #1865, #4689, #6779, #7527, #7623, #1154 ),
 .UNSPECIFIED., .F., .F. ) 
 B_SPLINE_CURVE_WITH_KNOTS ( ( 3, 2, 2, 2, 3 ),
 ( 0.5625000000000000000, 0.5694444444444444198, 0.5833333333333333703, 0.5972222222222222099, 0.6041666666666666297 ),
 .UNSPECIFIED. ) 
 CURVE ( )  GEOMETRIC_REPRESENTATION_ITEM ( )  RATIONAL_B_SPLINE_CURVE ( ( 0.9330127018922194093, 0.9330127018922194093, 1.000000000000000000, 0.8660254037844387076, 1.000000000000000000, 0.8660254037844387076, 1.000000000000000000, 0.9330127018922198534, 0.9330127018922192983 ) ) 
 REPRESENTATION_ITEM ( '' )  );
#8782 = CARTESIAN_POINT ( 'NONE',  ( -2.625000000000000444, -28.47916666598386826, -4.546633369868303021 ) ) ;
#8783 = CARTESIAN_POINT ( 'NONE',  ( -1.406733260263391960, -27.63616454900183328, 5.250000000000000000 ) ) ;
#8784 = CARTESIAN_POINT ( 'NONE',  ( -3.492485675378535603, -1.749340926099361093, -1.467888652719048670 ) ) ;
#8785 = DIRECTION ( 'NONE',  ( 0.000000000000000000, 0.000000000000000000, 1.000000000000000000 ) ) ;
#8786 = DIRECTION ( 'NONE',  ( 0.000000000000000000, 1.000000000000000000, 0.000000000000000000 ) ) ;
#8787 = CARTESIAN_POINT ( 'NONE',  ( 5.385316468750000141, -27.70312499965860198, -6.595110575850215044E-16 ) ) ;
#8788 = CARTESIAN_POINT ( 'NONE',  ( 4.000000000000000000, -7.449340926099361937, 0.01814118441321914063 ) ) ;
#8789 = CARTESIAN_POINT ( 'NONE',  ( -5.250000000000000888, -27.35416666666666430, 3.031088913245533423 ) ) ;
#8790 = ORIENTED_EDGE ( 'NONE', *, *, #8067, .T. ) ;
#8791 = CARTESIAN_POINT ( 'NONE',  ( 5.385316468750001029, -28.47395833299193413, 3.109213912904135846 ) ) ;
#8792 = CARTESIAN_POINT ( 'NONE',  ( -1.260781871532431708, -7.450659073900640195, -2.992485675378564469 ) ) ;
#8793 = ORIENTED_EDGE ( 'NONE', *, *, #1794, .F. ) ;
#8794 = CARTESIAN_POINT ( 'NONE',  ( -2.624999999999998668, -27.41666666666666430, -4.546633369868303021 ) ) ;
#8795 = CARTESIAN_POINT ( 'NONE',  ( -2.487701488670202910, -4.350659073900638774, -2.462045979635629767 ) ) ;
#8796 = VERTEX_POINT ( 'NONE', #381 ) ;
#8797 = ADVANCED_FACE ( 'NONE', ( #3143, #8108 ), #4666, .T. ) ;
#8798 = ORIENTED_EDGE ( 'NONE', *, *, #1859, .T. ) ;
#8799 = CARTESIAN_POINT ( 'NONE',  ( 2.557341765624996821, -29.40104166700806232, 4.429445870380401828 ) ) ;
#8800 = CARTESIAN_POINT ( 'NONE',  ( -3.507514324621464397, -1.949340926099361271, 1.431606283892619347 ) ) ;
#8801 = CARTESIAN_POINT ( 'NONE',  ( 1.406733260263394625, -28.47991455036742892, -5.250000000000000000 ) ) ;
#8802 = CARTESIAN_POINT ( 'NONE',  ( -2.557341765624999042, -28.58854166700806587, -4.429445870380400052 ) ) ;
#8803 = ORIENTED_EDGE ( 'NONE', *, *, #761, .F. ) ;
#8804 = VECTOR ( 'NONE', #5530, 1000.000000000000000 ) ;
#8805 = AXIS2_PLACEMENT_3D ( 'NONE', #4621, #8890, #3883 ) ;
#8806 = CARTESIAN_POINT ( 'NONE',  ( 0.000000000000000000, 1.000000000000000000, 0.000000000000000000 ) ) ;
#8807 = CARTESIAN_POINT ( 'NONE',  ( 5.114683531249999859, -27.58854166700806587, -2.952963913586932776 ) ) ;
#8808 = VERTEX_POINT ( 'NONE', #6755 ) ;
#8809 = VECTOR ( 'NONE', #8232, 1000.000000000000000 ) ;
#8810 = CARTESIAN_POINT ( 'NONE',  ( 2.624999999999998668, -27.83333333333333215, -4.546633369868303021 ) ) ;
#8811 = CARTESIAN_POINT ( 'NONE',  ( 5.385316468750000141, -28.48437499965860198, -6.595110575850215044E-16 ) ) ;
#8812 = CARTESIAN_POINT ( 'NONE',  ( -1.638713065079245634, -6.450659073900638418, 4.007514324621432422 ) ) ;
#8813=STYLED_ITEM('',(#9218),#5399);
#8814 = CARTESIAN_POINT ( 'NONE',  ( -5.385316468750000141, -28.10937499965860198, 0.000000000000000000 ) ) ;
#8815 = ORIENTED_EDGE ( 'NONE', *, *, #6120, .F. ) ;
#8816 = CARTESIAN_POINT ( 'NONE',  ( -2.624999999999998668, -29.91666666666666430, -4.546633369868303021 ) ) ;
#8817 = DIRECTION ( 'NONE',  ( -0.000000000000000000, -1.000000000000000000, -0.000000000000000000 ) ) ;
#8818 = EDGE_CURVE ( 'NONE', #2168, #8837, #8053, .T. ) ;
#8819 = CARTESIAN_POINT ( 'NONE',  ( 5.385316468749999252, -28.46354166632526628, -3.109213912904139399 ) ) ;
#8820 = AXIS2_PLACEMENT_3D ( 'NONE', #4408, #6488, #1566 ) ;
#8821 = ORIENTED_EDGE ( 'NONE', *, *, #1077, .F. ) ;
#8822 = DIRECTION ( 'NONE',  ( 0.000000000000000000, 1.000000000000000000, 0.000000000000000000 ) ) ;
#8823 = CARTESIAN_POINT ( 'NONE',  ( 2.134148098076933397, -0.3506590739006394397, 2.108492589042352261 ) ) ;
#8824 = DIRECTION ( 'NONE',  ( 1.000000000000000000, 0.000000000000000000, 0.000000000000000000 ) ) ;
#8825 = PRODUCT_DEFINITION_SHAPE ( 'NONE', 'NONE',  #5115 ) ;
#8826 = CARTESIAN_POINT ( 'NONE',  ( 2.624999999999998668, -27.27083333265053611, -4.546633369868303021 ) ) ;
#8827 = CARTESIAN_POINT ( 'NONE',  ( 1.975475456537005874E-15, -27.68749999999999289, 5.250000000000000000 ) ) ;
#8828 = CARTESIAN_POINT ( 'NONE',  ( -1.431606283892620235, -4.749340926099363536, -3.507514324621463953 ) ) ;
#8829 = CARTESIAN_POINT ( 'NONE',  ( -5.114683531249999859, -29.75520833367473017, -2.952963913586935440 ) ) ;
#8830 = ORIENTED_EDGE ( 'NONE', *, *, #1730, .F. ) ;
#8831 = CARTESIAN_POINT ( 'NONE',  ( 5.385316468750000141, -28.45312499965860198, -6.595110575850215044E-16 ) ) ;
#8832 = CARTESIAN_POINT ( 'NONE',  ( 2.841254879263533262, -7.649340926099361226, -2.815599370228847320 ) ) ;
#8833 = CARTESIAN_POINT ( 'NONE',  ( -5.250000000000000000, -28.50000000000000000, 0.000000000000000000 ) ) ;
#8834 = ORIENTED_EDGE ( 'NONE', *, *, #4748, .T. ) ;
#8835 = CARTESIAN_POINT ( 'NONE',  ( -5.385316468749998364, -28.05729166632526983, 3.109213912904140287 ) ) ;
#8836 = CARTESIAN_POINT ( 'NONE',  ( 1.431606283892694842, -7.250659073900640017, -3.507514324621434199 ) ) ;
#8837 = VERTEX_POINT ( 'NONE', #1787 ) ;
#8838 = CARTESIAN_POINT ( 'NONE',  ( -5.250000000000000888, -27.85416666666666430, 3.031088913245532979 ) ) ;
#8839 = CARTESIAN_POINT ( 'NONE',  ( -3.492485675378566246, -1.450659073900639084, 1.467888652718973175 ) ) ;
#8840 = VERTEX_POINT ( 'NONE', #4620 ) ;
#8841 = CARTESIAN_POINT ( 'NONE',  ( 2.625000000000002220, -27.66666666666666430, 4.546633369868302132 ) ) ;
#8842 = VERTEX_POINT ( 'NONE', #2437 ) ;
#8843 = EDGE_CURVE ( 'NONE', #2470, #4857, #6095, .T. ) ;
#8844 = CARTESIAN_POINT ( 'NONE',  ( 2.557341765625000818, -29.06770833367473017, -4.429445870380400052 ) ) ;
#8845 = CARTESIAN_POINT ( 'NONE',  ( -2.108492589042306964, -4.849340926099359628, -2.134148098076978251 ) ) ;
#8846 = PLANE ( 'NONE',  #7870 ) ;
#8847 = DIRECTION ( 'NONE',  ( 1.000000000000000000, 0.000000000000000000, 0.000000000000000000 ) ) ;
#8848 = CARTESIAN_POINT ( 'NONE',  ( 5.114683531249998971, -28.19270833367473372, 2.952963913586936329 ) ) ;
#8849 = CARTESIAN_POINT ( 'NONE',  ( -1.926921503246612044, -5.459919674188128654E-16, 2.888980742429482884 ) ) ;
#8850 = CARTESIAN_POINT ( 'NONE',  ( -2.557341765624999042, -27.77604166700806587, -4.429445870380400052 ) ) ;
#8851 = B_SPLINE_CURVE_WITH_KNOTS ( 'NONE', 3,
 ( #5554, #1410, #6333, #8488, #4250, #7083, #705, #3554, #59, #6375, #5681, #2863, #15, #8528, #4976, #1980, #7831, #1449, #3597, #6421 ),
 .UNSPECIFIED., .F., .F.,
 ( 4, 2, 2, 2, 2, 2, 2, 2, 2, 4 ),
 ( 0.003307978161309543027, 0.003337183750601276089, 0.003366389339893009151, 0.003424800518476474841, 0.003541622875643406221, 0.003775267589977268981, 0.004242557018644994501, 0.005177135875980443808, 0.006111714733315892246, 0.007046293590651341553 ),
 .UNSPECIFIED. ) ;
#8852 = ORIENTED_EDGE ( 'NONE', *, *, #2084, .F. ) ;
#8853 = DIRECTION ( 'NONE',  ( 0.000000000000000000, 0.000000000000000000, 1.000000000000000000 ) ) ;
#8854 = CARTESIAN_POINT ( 'NONE',  ( -2.692658234375000514, -29.40104166632526983, -4.663820869356205989 ) ) ;
#8855 = CARTESIAN_POINT ( 'NONE',  ( 0.000000000000000000, 74.00000000000001421, 0.000000000000000000 ) ) ;
#8856 = CARTESIAN_POINT ( 'NONE',  ( -3.807688866302469071E-16, -29.42187499965860198, -6.218427825808274356 ) ) ;
#8857 = ORIENTED_EDGE ( 'NONE', *, *, #8471, .T. ) ;
#8858 = CARTESIAN_POINT ( 'NONE',  ( -9.180150650966086169E-15, -28.43750000000000000, 5.250000000000000000 ) ) ;
#8859 = CARTESIAN_POINT ( 'NONE',  ( 5.249999999999999112, -28.05208333401612819, 3.031088913245538308 ) ) ;
#8860 = CARTESIAN_POINT ( 'NONE',  ( 2.692658234374998738, -29.19270833299193413, -4.663820869356206877 ) ) ;
#8861 = ORIENTED_EDGE ( 'NONE', *, *, #2193, .F. ) ;
#8862 = CARTESIAN_POINT ( 'NONE',  ( -2.692658234375000514, -27.61979166632526628, -4.663820869356205989 ) ) ;
#8863 = CARTESIAN_POINT ( 'NONE',  ( -3.492485675378566246, 0.1493409260993610876, 1.467888652718973397 ) ) ;
#8864 = DIRECTION ( 'NONE',  ( 0.000000000000000000, 0.000000000000000000, -1.000000000000000000 ) ) ;
#8865 = COLOUR_RGB ( '',0.8941176470588234615, 0.8941176470588234615, 0.8941176470588234615 ) ;
#8866 = CARTESIAN_POINT ( 'NONE',  ( 0.000000000000000000, 73.00000000000001421, 0.000000000000000000 ) ) ;
#8867 = DIRECTION ( 'NONE',  ( 0.000000000000000000, -1.000000000000000000, 0.000000000000000000 ) ) ;
#8868 = CARTESIAN_POINT ( 'NONE',  ( -1.467888652719046449, -5.349340926099361404, 3.492485675378535603 ) ) ;
#8869 = CARTESIAN_POINT ( 'NONE',  ( 2.557341765624996821, -29.40104166700806232, 4.429445870380401828 ) ) ;
#8870 = VERTEX_POINT ( 'NONE', #4555 ) ;
#8871 = PRODUCT_CONTEXT ( 'NONE', #7965, 'mechanical' ) ;
#8872 = CARTESIAN_POINT ( 'NONE',  ( 1.142306659890740623E-15, -29.26562499965860198, 6.218427825808274356 ) ) ;
#8873 = CARTESIAN_POINT ( 'NONE',  ( -1.674995433905599462, -3.749340926099360871, 3.992485675378533383 ) ) ;
#8874 = DIRECTION ( 'NONE',  ( 0.000000000000000000, -1.000000000000000000, 0.000000000000000000 ) ) ;
#8875 = CARTESIAN_POINT ( 'NONE',  ( -2.692658234374996518, -28.53645833299193413, 4.663820869356208654 ) ) ;
#8876 = CARTESIAN_POINT ( 'NONE',  ( -3.492485675378566246, -3.050659073900638507, 1.467888652718973397 ) ) ;
#8877 = ORIENTED_EDGE ( 'NONE', *, *, #2827, .F. ) ;
#8878 = CARTESIAN_POINT ( 'NONE',  ( -2.625000000000002220, -27.83333333333333215, 4.546633369868302132 ) ) ;
#8879 = CARTESIAN_POINT ( 'NONE',  ( -1.467888652718973841, -7.450659073900639306, -3.492485675378565801 ) ) ;
#8880 = CARTESIAN_POINT ( 'NONE',  ( 3.507514324621434199, -3.650659073900639484, 1.431606283892693066 ) ) ;
#8881 = ADVANCED_FACE ( 'NONE', ( #7247 ), #7951, .T. ) ;
#8882 = VERTEX_POINT ( 'NONE', #5807 ) ;
#8883 =( NAMED_UNIT ( * ) SI_UNIT ( $, .STERADIAN. ) SOLID_ANGLE_UNIT ( ) );
#8884 = CARTESIAN_POINT ( 'NONE',  ( -5.250000000000000000, -27.25000000000000000, 0.000000000000000000 ) ) ;
#8885 = ORIENTED_EDGE ( 'NONE', *, *, #7988, .T. ) ;
#8886 = VECTOR ( 'NONE', #1475, 1000.000000000000000 ) ;
#8887 = CARTESIAN_POINT ( 'NONE',  ( 2.557341765625000818, -29.31770833367473017, -4.429445870380400052 ) ) ;
#8888 = CARTESIAN_POINT ( 'NONE',  ( 2.134148098076978251, -2.849340926099362292, -2.108492589042307408 ) ) ;
#8889 = CARTESIAN_POINT ( 'NONE',  ( -3.500000000000000000, -7.750659073900639129, 0.01814118441314012051 ) ) ;
#8890 = DIRECTION ( 'NONE',  ( 0.000000000000000000, 1.000000000000000000, 0.000000000000000000 ) ) ;
#8891 = CARTESIAN_POINT ( 'NONE',  ( 2.557341765624996821, -28.71354166700806587, 4.429445870380401828 ) ) ;
#8892 = EDGE_CURVE ( 'NONE', #3365, #6742, #2225, .T. ) ;
#8893 = CARTESIAN_POINT ( 'NONE',  ( -1.406733260263385521, -27.85491455036742536, 5.250000000000006217 ) ) ;
#8894 = DIRECTION ( 'NONE',  ( 1.000000000000000000, 0.000000000000000000, 0.000000000000000000 ) ) ;
#8895 = VECTOR ( 'NONE', #2745, 1000.000000000000000 ) ;
#8896 = ORIENTED_EDGE ( 'NONE', *, *, #3394, .F. ) ;
#8897 = CARTESIAN_POINT ( 'NONE',  ( 0.000000000000000000, -30.00000000000000000, 0.000000000000000000 ) ) ;
#8898 = CARTESIAN_POINT ( 'NONE',  ( -2.692658234374996518, -28.81770833299193413, 4.663820869356208654 ) ) ;
#8899 = CARTESIAN_POINT ( 'NONE',  ( -5.385316468750000141, -29.60937499965859843, 0.000000000000000000 ) ) ;
#8900 = PRESENTATION_LAYER_ASSIGNMENT (  '', '', ( #2525 ) ) ;
#8901 = CARTESIAN_POINT ( 'NONE',  ( 4.000000000000000000, -7.449340926099361937, 0.01814118441321914063 ) ) ;
#8902 = ORIENTED_EDGE ( 'NONE', *, *, #79, .F. ) ;
#8903 = AXIS2_PLACEMENT_3D ( 'NONE', #4263, #3481, #6306 ) ;
#8904 = DIRECTION ( 'NONE',  ( 0.000000000000000000, 0.000000000000000000, 1.000000000000000000 ) ) ;
#8905 = CARTESIAN_POINT ( 'NONE',  ( -1.113604000661152470E-15, -27.84375000068279604, 6.062177826491070398 ) ) ;
#8906 = CARTESIAN_POINT ( 'NONE',  ( -2.692658234374996518, -29.81770833299193413, 4.663820869356208654 ) ) ;
#8907 = AXIS2_PLACEMENT_3D ( 'NONE', #5456, #8301, #9124 ) ;
#8908 = EDGE_LOOP ( 'NONE', ( #4901, #4570, #4673, #3213 ) ) ;
#8909 = CARTESIAN_POINT ( 'NONE',  ( -3.807688866302469071E-16, -28.39062499965860553, -6.218427825808274356 ) ) ;
#8910 = CARTESIAN_POINT ( 'NONE',  ( 3.507514324621434199, -0.4506590739006390844, 1.431606283892693066 ) ) ;
#8911 = DIRECTION ( 'NONE',  ( 0.000000000000000000, 0.000000000000000000, -1.000000000000000000 ) ) ;
#8912 = VECTOR ( 'NONE', #734, 1000.000000000000000 ) ;
#8913 = EDGE_CURVE ( 'NONE', #1752, #6843, #8609, .T. ) ;
#8914 = CARTESIAN_POINT ( 'NONE',  ( -2.624999999999998668, -28.91666666666666785, -4.546633369868303021 ) ) ;
#8915 = CYLINDRICAL_SURFACE ( 'NONE', #8230, 5.250000000000000000 ) ;
#8916 = AXIS2_PLACEMENT_3D ( 'NONE', #910, #1002, #5975 ) ;
#8917 = DIRECTION ( 'NONE',  ( -0.000000000000000000, -1.000000000000000000, -0.000000000000000000 ) ) ;
#8918 = EDGE_LOOP ( 'NONE', ( #5230, #6660, #6071, #5995 ) ) ;
#8919 = DIRECTION ( 'NONE',  ( 0.000000000000000000, 0.000000000000000000, 1.000000000000000000 ) ) ;
#8920 = CARTESIAN_POINT ( 'NONE',  ( -3.500000000000000000, -8.249340926099360871, -0.01814118441321344033 ) ) ;
#8921 = CARTESIAN_POINT ( 'NONE',  ( -5.249999999999999112, -28.02083333333333215, -3.031088913245534755 ) ) ;
#8922 = CARTESIAN_POINT ( 'NONE',  ( 2.692658234375002735, -28.74479166632526628, 4.663820869356205101 ) ) ;
#8923 = CARTESIAN_POINT ( 'NONE',  ( -1.467888652718973619, -7.450659073900638418, -3.492485675378565801 ) ) ;
#8924 = AXIS2_PLACEMENT_3D ( 'NONE', #5466, #6769, #7472 ) ;
#8925 = ORIENTED_EDGE ( 'NONE', *, *, #4489, .F. ) ;
#8926 = CARTESIAN_POINT ( 'NONE',  ( -2.624999999999998668, -27.19791666734946389, -4.546633369868303021 ) ) ;
#8927 = DIRECTION ( 'NONE',  ( 0.000000000000000000, 0.000000000000000000, 1.000000000000000000 ) ) ;
#8928 = CARTESIAN_POINT ( 'NONE',  ( 5.114683531250000748, -27.17187500034139802, 0.000000000000000000 ) ) ;
#8929 = VERTEX_POINT ( 'NONE', #3862 ) ;
#8930 = CARTESIAN_POINT ( 'NONE',  ( 5.250000000000000000, -28.12500000000000000, -6.429395695523604153E-16 ) ) ;
#8931 = EDGE_LOOP ( 'NONE', ( #3815, #2761 ) ) ;
#8932 = CARTESIAN_POINT ( 'NONE',  ( -5.114683531250000748, -29.48437500034139802, -6.263680815196995234E-16 ) ) ;
#8933 = CARTESIAN_POINT ( 'NONE',  ( 1.260781871532495657, -4.549340926099363358, -2.992485675378538268 ) ) ;
#8934 = CARTESIAN_POINT ( 'NONE',  ( 2.033577675846918216E-14, -28.06249999999999645, 5.250000000000000888 ) ) ;
#8935 = CARTESIAN_POINT ( 'NONE',  ( -5.114683531250000748, -29.29687500034139802, -6.263680815196995234E-16 ) ) ;
#8936 = CARTESIAN_POINT ( 'NONE',  ( 5.249999999999999112, -29.22916666666666785, -3.031088913245534755 ) ) ;
#8937 = DIRECTION ( 'NONE',  ( 0.000000000000000000, 0.000000000000000000, 1.000000000000000000 ) ) ;
#8938 = CARTESIAN_POINT ( 'NONE',  ( 5.249999999999997335, -27.02083333333334281, 3.031088913245538308 ) ) ;
#8939 = CARTESIAN_POINT ( 'NONE',  ( 5.114683531250000748, -29.42187500034139802, 0.000000000000000000 ) ) ;
#8940 =( BOUNDED_CURVE ( )  B_SPLINE_CURVE ( 2, ( #2815, #3462, #9037, #6372, #4246, #4932, #1977, #8485, #2062 ),
 .UNSPECIFIED., .F., .F. ) 
 B_SPLINE_CURVE_WITH_KNOTS ( ( 3, 2, 2, 2, 3 ),
 ( 0.4375000000000000000, 0.4444444444444444198, 0.4583333333333333148, 0.4722222222222222099, 0.4791666666666666852 ),
 .UNSPECIFIED. ) 
 CURVE ( )  GEOMETRIC_REPRESENTATION_ITEM ( )  RATIONAL_B_SPLINE_CURVE ( ( 0.9330127018922194093, 0.9330127018922194093, 1.000000000000000000, 0.8660254037844387076, 1.000000000000000000, 0.8660254037844387076, 1.000000000000000000, 0.9330127018922190762, 0.9330127018922194093 ) ) 
 REPRESENTATION_ITEM ( '' )  );
#8941 = ADVANCED_FACE ( 'NONE', ( #1717 ), #4372, .F. ) ;
#8942 = CYLINDRICAL_SURFACE ( 'NONE', #1857, 5.250000000000000000 ) ;
#8943 = CARTESIAN_POINT ( 'NONE',  ( -3.807688866302469071E-16, -28.17187499965860198, -6.218427825808274356 ) ) ;
#8944 = CARTESIAN_POINT ( 'NONE',  ( -2.625000000000002220, -29.11458333401613174, 4.546633369868302132 ) ) ;
#8945 = CARTESIAN_POINT ( 'NONE',  ( -3.500000000000000000, 0.000000000000000000, -3.665958595716611867E-14 ) ) ;
#8946 = CARTESIAN_POINT ( 'NONE',  ( 5.385316468749999252, -28.96354166632526983, -3.109213912904139399 ) ) ;
#8947 = CARTESIAN_POINT ( 'NONE',  ( -2.487701488670255312, -2.049340926099361582, 2.462045979635577808 ) ) ;
#8948 = VERTEX_POINT ( 'NONE', #1574 ) ;
#8949 =( REPRESENTATION_RELATIONSHIP ('NONE','NONE', #735, #2490 ) REPRESENTATION_RELATIONSHIP_WITH_TRANSFORMATION ( #7059 )SHAPE_REPRESENTATION_RELATIONSHIP( ) );
#8950 = CARTESIAN_POINT ( 'NONE',  ( 5.249999999999999112, -28.35416666666666785, -3.031088913245536975 ) ) ;
#8951 = CARTESIAN_POINT ( 'NONE',  ( -5.250000000000000000, -27.65625000068279959, -6.429395695523604153E-16 ) ) ;
#8952 = CARTESIAN_POINT ( 'NONE',  ( -3.807688866302469071E-16, -29.42187499965860198, -6.218427825808274356 ) ) ;
#8953 = VECTOR ( 'NONE', #6076, 1000.000000000000000 ) ;
#8954 = EDGE_CURVE ( 'NONE', #6870, #5024, #5945, .T. ) ;
#8955 = ORIENTED_EDGE ( 'NONE', *, *, #313, .F. ) ;
#8956 = CARTESIAN_POINT ( 'NONE',  ( -5.385316468750000141, -28.07812499965860198, 0.000000000000000000 ) ) ;
#8957 = CARTESIAN_POINT ( 'NONE',  ( -2.487701488670202910, -2.750659073900639129, -2.462045979635629767 ) ) ;
#8958 = FACE_OUTER_BOUND ( 'NONE', #7818, .T. ) ;
#8959 = EDGE_CURVE ( 'NONE', #6175, #2431, #7651, .T. ) ;
#8960 = CIRCLE ( 'NONE', #5553, 1.749999999999999778 ) ;
#8961 = CARTESIAN_POINT ( 'NONE',  ( 9.180150650966086169E-15, -28.81250000000000000, 5.250000000000000000 ) ) ;
#8962 = CARTESIAN_POINT ( 'NONE',  ( -2.624999999999996891, -28.39583333265053611, 4.546633369868304797 ) ) ;
#8963 = CYLINDRICAL_SURFACE ( 'NONE', #8327, 2.500000000000000444 ) ;
#8964 = CARTESIAN_POINT ( 'NONE',  ( 3.673940397442059375E-16, -47.00000000000000000, 2.999999999999999556 ) ) ;
#8965 = ORIENTED_EDGE ( 'NONE', *, *, #7129, .F. ) ;
#8966 = APPLICATION_PROTOCOL_DEFINITION ( 'draft international standard', 'automotive_design', 1998, #3735 ) ;
#8967 = CARTESIAN_POINT ( 'NONE',  ( 2.692658234375002735, -28.99479166632526983, 4.663820869356205101 ) ) ;
#8968 = CARTESIAN_POINT ( 'NONE',  ( 2.462045979635577364, -7.249340926099360871, 2.487701488670255312 ) ) ;
#8969 = DIRECTION ( 'NONE',  ( 0.000000000000000000, 1.000000000000000000, 0.000000000000000000 ) ) ;
#8970 = CARTESIAN_POINT ( 'NONE',  ( 5.385316468750000141, -29.20312499965859843, -6.595110575850215044E-16 ) ) ;
#8971 = CARTESIAN_POINT ( 'NONE',  ( -1.467888652718973619, -2.650659073900639040, -3.492485675378565801 ) ) ;
#8972 = ORIENTED_EDGE ( 'NONE', *, *, #6696, .T. ) ;
#8973 = CARTESIAN_POINT ( 'NONE',  ( -5.250000000000000000, -27.12500000000000000, -6.429395695523604153E-16 ) ) ;
#8974 = PRODUCT_DEFINITION_CONTEXT ( 'detailed design', #2904, 'design' ) ;
#8975 = CARTESIAN_POINT ( 'NONE',  ( 0.000000000000000000, 70.00000000000000000, -3.000000000000000444 ) ) ;
#8976 = CARTESIAN_POINT ( 'NONE',  ( -2.462045979635629323, -1.550659073900639173, 2.487701488670203798 ) ) ;
#8977 = ORIENTED_EDGE ( 'NONE', *, *, #513, .T. ) ;
#8978 =( NAMED_UNIT ( * ) PLANE_ANGLE_UNIT ( ) SI_UNIT ( $, .RADIAN. ) );
#8979 = CARTESIAN_POINT ( 'NONE',  ( -5.250000000000000000, -28.52083333333333215, -3.031088913245534755 ) ) ;
#8980 = EDGE_LOOP ( 'NONE', ( #2303, #45, #6892, #8861 ) ) ;
#8981 = CARTESIAN_POINT ( 'NONE',  ( -5.114683531250000748, -28.98437500034139802, -6.263680815196995234E-16 ) ) ;
#8982 = CARTESIAN_POINT ( 'NONE',  ( -3.000000000000000444, -5.049340926099361582, -0.01814118441320822922 ) ) ;
#8983 = DIRECTION ( 'NONE',  ( 0.000000000000000000, 1.000000000000000000, 0.000000000000000000 ) ) ;
#8984 = CARTESIAN_POINT ( 'NONE',  ( 2.557341765624996821, -27.21354166700806587, 4.429445870380401828 ) ) ;
#8985 = CARTESIAN_POINT ( 'NONE',  ( 6.429395695523604153E-16, -27.00000000000000000, 5.250000000000000000 ) ) ;
#8986 = CARTESIAN_POINT ( 'NONE',  ( 2.557341765625000818, -27.56770833367473017, -4.429445870380400052 ) ) ;
#8987 = DIRECTION ( 'NONE',  ( 0.000000000000000000, 1.000000000000000000, 0.000000000000000000 ) ) ;
#8988 = CARTESIAN_POINT ( 'NONE',  ( 5.114683531249998971, -29.19270833367473017, 2.952963913586936329 ) ) ;
#8989 = CARTESIAN_POINT ( 'NONE',  ( 0.000000000000000000, 81.00000000000001421, 0.000000000000000000 ) ) ;
#8990 = CARTESIAN_POINT ( 'NONE',  ( -5.385316468749998364, -28.83854166632527338, 3.109213912904140287 ) ) ;
#8991 = CARTESIAN_POINT ( 'NONE',  ( 0.000000000000000000, -30.00000000000000000, 0.000000000000000000 ) ) ;
#8992 = SURFACE_STYLE_FILL_AREA ( #2494 ) ;
#8993 = CARTESIAN_POINT ( 'NONE',  ( -5.385316468750000141, -28.85937499965860198, 0.000000000000000000 ) ) ;
#8994 = CARTESIAN_POINT ( 'NONE',  ( -2.815599370228846876, -8.049340926099359805, -2.841254879263533262 ) ) ;
#8995 = CARTESIAN_POINT ( 'NONE',  ( 3.492485675378536047, -2.549340926099360694, 1.467888652719046672 ) ) ;
#8996 = ORIENTED_EDGE ( 'NONE', *, *, #9163, .T. ) ;
#8997 = CARTESIAN_POINT ( 'NONE',  ( 6.972266317189433020E-16, -29.21875000068279249, -5.250000000000000000 ) ) ;
#8998 = CARTESIAN_POINT ( 'NONE',  ( -5.250000000000000000, -28.67708333401612819, -3.031088913245536531 ) ) ;
#8999 =( BOUNDED_CURVE ( )  B_SPLINE_CURVE ( 2, ( #5810, #6291, #2772, #9083, #8648, #8352, #6330, #4807, #2280 ),
 .UNSPECIFIED., .F., .F. ) 
 B_SPLINE_CURVE_WITH_KNOTS ( ( 3, 2, 2, 2, 3 ),
 ( 0.5625000000000000000, 0.5694444444444444198, 0.5833333333333333703, 0.5972222222222222099, 0.6041666666666667407 ),
 .UNSPECIFIED. ) 
 CURVE ( )  GEOMETRIC_REPRESENTATION_ITEM ( )  RATIONAL_B_SPLINE_CURVE ( ( 0.9330127018922194093, 0.9330127018922194093, 1.000000000000000000, 0.8660254037844387076, 1.000000000000000000, 0.8660254037844387076, 1.000000000000000000, 0.9330127018922187432, 0.9330127018922192983 ) ) 
 REPRESENTATION_ITEM ( '' )  );
#9000 = CARTESIAN_POINT ( 'NONE',  ( -5.385316468750000141, -29.85937499965859843, 0.000000000000000000 ) ) ;
#9001 = EDGE_CURVE ( 'NONE', #7379, #3780, #7048, .T. ) ;
#9002 = ORIENTED_EDGE ( 'NONE', *, *, #9010, .T. ) ;
#9003 = CARTESIAN_POINT ( 'NONE',  ( 5.385316468750000141, -28.45312499965860198, -6.595110575850215044E-16 ) ) ;
#9004 = CARTESIAN_POINT ( 'NONE',  ( 0.01814118441313990887, -1.750659073900638907, 3.500000000000000000 ) ) ;
#9005 = CARTESIAN_POINT ( 'NONE',  ( 5.249999999999999112, -29.76041666734946034, -3.031088913245534755 ) ) ;
#9006 = EDGE_CURVE ( 'NONE', #6014, #4009, #5641, .T. ) ;
#9007 = CARTESIAN_POINT ( 'NONE',  ( 4.898587196589412829E-16, 81.00000000000001421, 4.000000000000000000 ) ) ;
#9008 = CYLINDRICAL_SURFACE ( 'NONE', #2430, 5.250000000000000000 ) ;
#9009 = CARTESIAN_POINT ( 'NONE',  ( 2.624999999999996891, -28.07291666734946389, 4.546633369868304797 ) ) ;
#9010 = EDGE_CURVE ( 'NONE', #7186, #6937, #7297, .T. ) ;
#9011 = FACE_OUTER_BOUND ( 'NONE', #3451, .T. ) ;
#9012 = CARTESIAN_POINT ( 'NONE',  ( 0.000000000000000000, -9.000000000000000000, 0.000000000000000000 ) ) ;
#9013 = APPLICATION_PROTOCOL_DEFINITION ( 'draft international standard', 'automotive_design', 1998, #4961 ) ;
#9014 = CARTESIAN_POINT ( 'NONE',  ( -3.807688866302469071E-16, -28.89062499965860198, -6.218427825808274356 ) ) ;
#9015 = CARTESIAN_POINT ( 'NONE',  ( 1.467888652719048226, -7.749340926099361759, -3.492485675378536047 ) ) ;
#9016 = CARTESIAN_POINT ( 'NONE',  ( -9.180150650966086169E-15, -28.62499999931720396, 5.250000000000000000 ) ) ;
#9017 = CARTESIAN_POINT ( 'NONE',  ( 2.692658234374998738, -29.66145833299193413, -4.663820869356206877 ) ) ;
#9018 = CARTESIAN_POINT ( 'NONE',  ( 1.467888652718972731, -6.650659073900639484, 3.492485675378566246 ) ) ;
#9019 = ORIENTED_EDGE ( 'NONE', *, *, #3658, .T. ) ;
#9020 = LINE ( 'NONE', #7540, #3614 ) ;
#9021 = DIRECTION ( 'NONE',  ( 0.000000000000000000, 1.000000000000000000, 0.000000000000000000 ) ) ;
#9022 = CARTESIAN_POINT ( 'NONE',  ( 2.462045979635629767, -5.550659073900639839, -2.487701488670203354 ) ) ;
#9023 = STYLED_ITEM ( 'NONE', ( #7639 ), #2088 ) ;
#9024 = ORIENTED_EDGE ( 'NONE', *, *, #5379, .F. ) ;
#9025 = CARTESIAN_POINT ( 'NONE',  ( 5.250000000000000000, -28.10416666666666430, -3.031088913245536531 ) ) ;
#9026 = CARTESIAN_POINT ( 'NONE',  ( 2.557341765625000818, -27.06770833367473017, -4.429445870380400052 ) ) ;
#9027 = CARTESIAN_POINT ( 'NONE',  ( 2.992485675378538712, -0.9493409260993616039, 1.260781871532494103 ) ) ;
#9028 = CARTESIAN_POINT ( 'NONE',  ( 6.429395695523604153E-16, -30.00000000000000000, -5.250000000000000000 ) ) ;
#9029 = CARTESIAN_POINT ( 'NONE',  ( -1.084901341431563923E-15, -27.73437500034139802, 5.905927827173866440 ) ) ;
#9030 = PRODUCT_DEFINITION_FORMATION_WITH_SPECIFIED_SOURCE ( 'ANY', '', #5066, .NOT_KNOWN. ) ;
#9031 = PLANE ( 'NONE',  #2741 ) ;
#9032 = ADVANCED_FACE ( 'NONE', ( #228 ), #3076, .T. ) ;
#9033 = ADVANCED_FACE ( 'NONE', ( #6639, #268 ), #3121, .F. ) ;
#9034 = CARTESIAN_POINT ( 'NONE',  ( 5.114683531250000748, -29.42187500034139802, 0.000000000000000000 ) ) ;
#9035 = CARTESIAN_POINT ( 'NONE',  ( -5.250000000000000000, -28.37499999999999645, -6.429395695523604153E-16 ) ) ;
#9036 = CARTESIAN_POINT ( 'NONE',  ( 5.114683531249999859, -29.15104166700806232, -2.952963913586932776 ) ) ;
#9037 = CARTESIAN_POINT ( 'NONE',  ( -2.624999999999998668, -28.44791666734946389, -4.546633369868303021 ) ) ;
#9038 = CARTESIAN_POINT ( 'NONE',  ( 5.250000000000000000, -29.31249999931720041, -6.429395695523604153E-16 ) ) ;
#9039 = CARTESIAN_POINT ( 'NONE',  ( 5.385316468750001029, -30.00520833299193768, 3.109213912904134958 ) ) ;
#9040 = CARTESIAN_POINT ( 'NONE',  ( 6.429395695523604153E-16, -30.00000000000000000, -5.250000000000000000 ) ) ;
#9041 = CARTESIAN_POINT ( 'NONE',  ( -5.385316468750001029, -29.38020833299193413, -3.109213912904136734 ) ) ;
#9042 = CARTESIAN_POINT ( 'NONE',  ( 2.487701488670255756, -1.249340926099361093, -2.462045979635577364 ) ) ;
#9043 = CARTESIAN_POINT ( 'NONE',  ( -3.507514324621464397, -1.949340926099361271, 1.431606283892619347 ) ) ;
#9044 = ORIENTED_EDGE ( 'NONE', *, *, #2304, .T. ) ;
#9045 = CARTESIAN_POINT ( 'NONE',  ( 5.250000000000000888, -28.39583333333333215, 3.031088913245533423 ) ) ;
#9046 = CARTESIAN_POINT ( 'NONE',  ( 2.625000000000000444, -27.73958333401612819, -4.546633369868303021 ) ) ;
#9047 = CARTESIAN_POINT ( 'NONE',  ( 5.385316468749999252, -29.21354166632526628, -3.109213912904139399 ) ) ;
#9048 = ORIENTED_EDGE ( 'NONE', *, *, #8523, .T. ) ;
#9049 = VECTOR ( 'NONE', #1333, 1000.000000000000000 ) ;
#9050 = CARTESIAN_POINT ( 'NONE',  ( 5.385316468750000141, -27.95312499965860198, -6.595110575850215044E-16 ) ) ;
#9051 = CARTESIAN_POINT ( 'NONE',  ( 1.467888652718972731, -1.850659073900638996, 3.492485675378566246 ) ) ;
#9052 = CARTESIAN_POINT ( 'NONE',  ( 1.406733260263391960, -29.55133545031537068, 5.250000000000000000 ) ) ;
#9053 = PRODUCT_DEFINITION_SHAPE ( 'NONE', 'NONE',  #9189 ) ;
#9054 = DIRECTION ( 'NONE',  ( 0.000000000000000000, 1.000000000000000000, 0.000000000000000000 ) ) ;
#9055 = CARTESIAN_POINT ( 'NONE',  ( 0.000000000000000000, 76.00000000000000000, 6.250000000000000000 ) ) ;
#9056 = CIRCLE ( 'NONE', #136, 4.250000000000000000 ) ;
#9057 = CARTESIAN_POINT ( 'NONE',  ( 5.249999999999997335, -28.05208333401612819, 3.031088913245538308 ) ) ;
#9058 = CARTESIAN_POINT ( 'NONE',  ( 2.557341765625000818, -28.06770833367473017, -4.429445870380400052 ) ) ;
#9059 = CARTESIAN_POINT ( 'NONE',  ( 1.045839947578414884E-14, -28.24999999931720041, -5.250000000000000000 ) ) ;
#9060 = CONICAL_SURFACE ( 'NONE', #5199, 6.250000000000002665, 0.1221730476396033355 ) ;
#9061 = APPLICATION_PROTOCOL_DEFINITION ( 'draft international standard', 'automotive_design', 1998, #5270 ) ;
#9062 = CARTESIAN_POINT ( 'NONE',  ( 1.142306659890740623E-15, -29.51562499965859487, 6.218427825808274356 ) ) ;
#9063 = CARTESIAN_POINT ( 'NONE',  ( 0.01814118441321408565, -6.249340926099360871, -3.500000000000000000 ) ) ;
#9064 = EDGE_CURVE ( 'NONE', #8178, #627, #2060, .T. ) ;
#9065 = CARTESIAN_POINT ( 'NONE',  ( 2.624999999999998668, -28.52083333265053611, -4.546633369868303021 ) ) ;
#9066 = CARTESIAN_POINT ( 'NONE',  ( 2.692658234375002735, -29.24479166632526983, 4.663820869356205101 ) ) ;
#9067 = CARTESIAN_POINT ( 'NONE',  ( 3.992485675378568910, -0.6506590739006385959, -1.674995433905514863 ) ) ;
#9068 = CARTESIAN_POINT ( 'NONE',  ( 5.250000000000000000, -28.99999999999999645, 0.000000000000000000 ) ) ;
#9069 = CIRCLE ( 'NONE', #4176, 2.750000000000000000 ) ;
#9070 = DIRECTION ( 'NONE',  ( 0.000000000000000000, 1.000000000000000000, 0.000000000000000000 ) ) ;
#9071 = ORIENTED_EDGE ( 'NONE', *, *, #3103, .T. ) ;
#9072 = CARTESIAN_POINT ( 'NONE',  ( -5.250000000000000000, -28.75000000000000000, 0.000000000000000000 ) ) ;
#9073 = ADVANCED_FACE ( 'NONE', ( #5507 ), #4157, .T. ) ;
#9074 = CIRCLE ( 'NONE', #8903, 2.786798956483056422 ) ;
#9075 = CARTESIAN_POINT ( 'NONE',  ( 2.557341765624996821, -27.40104166700806587, 4.429445870380401828 ) ) ;
#9076 = CARTESIAN_POINT ( 'NONE',  ( -3.000000000000000444, -8.249340926099360871, -0.01814118441320822922 ) ) ;
#9077 = CARTESIAN_POINT ( 'NONE',  ( -5.250000000000000888, -29.85416666666666785, 3.031088913245532979 ) ) ;
#9078 = CARTESIAN_POINT ( 'NONE',  ( -2.033577675846918216E-14, -29.93750000000000355, 5.250000000000000888 ) ) ;
#9079 =( BOUNDED_CURVE ( )  B_SPLINE_CURVE ( 2, ( #416, #4745, #8926, #5487, #4834, #7680, #6145, #4057, #4791 ),
 .UNSPECIFIED., .F., .T. ) 
 B_SPLINE_CURVE_WITH_KNOTS ( ( 3, 2, 2, 2, 3 ),
 ( 0.8541666666666666297, 0.8611111111111111605, 0.8750000000000000000, 0.8888888888888888395, 0.8958333333333333703 ),
 .UNSPECIFIED. ) 
 CURVE ( )  GEOMETRIC_REPRESENTATION_ITEM ( )  RATIONAL_B_SPLINE_CURVE ( ( 0.9330127018922192983, 0.9330127018922187432, 1.000000000000000000, 0.8660254037844387076, 1.000000000000000000, 0.8660254037844387076, 1.000000000000000000, 0.9330127018922187432, 0.9330127018922192983 ) ) 
 REPRESENTATION_ITEM ( '' )  );
#9080 = CARTESIAN_POINT ( 'NONE',  ( 3.616337804771879580E-16, -29.35937500034139802, -5.905927827173866440 ) ) ;
#9081 = DIRECTION ( 'NONE',  ( 0.000000000000000000, 0.000000000000000000, 1.000000000000000000 ) ) ;
#9082 = CARTESIAN_POINT ( 'NONE',  ( 2.557341765625000818, -29.13020833367473017, -4.429445870380400052 ) ) ;
#9083 = CARTESIAN_POINT ( 'NONE',  ( -5.249999999999997335, -28.72916666666666785, 3.031088913245538308 ) ) ;
#9084 = CARTESIAN_POINT ( 'NONE',  ( 2.624999999999998668, -29.27083333265053611, -4.546633369868303021 ) ) ;
#9085 = DIRECTION ( 'NONE',  ( 0.000000000000000000, -1.000000000000000000, 0.000000000000000000 ) ) ;
#9086 = CARTESIAN_POINT ( 'NONE',  ( 5.250000000000000000, -29.53125000068279604, 0.000000000000000000 ) ) ;
#9087 = CARTESIAN_POINT ( 'NONE',  ( 0.000000000000000000, 0.000000000000000000, 0.000000000000000000 ) ) ;
#9088 = CARTESIAN_POINT ( 'NONE',  ( 0.01814118441321408565, -3.049340926099361138, -3.500000000000000000 ) ) ;
#9089 = CARTESIAN_POINT ( 'NONE',  ( 1.638713065079161924, -5.549340926099361582, 4.007514324621467949 ) ) ;
#9090 = ORIENTED_EDGE ( 'NONE', *, *, #6017, .T. ) ;
#9091 = CARTESIAN_POINT ( 'NONE',  ( -1.406733260263384411, -28.98883544963257464, -5.250000000000006217 ) ) ;
#9092 = CARTESIAN_POINT ( 'NONE',  ( 5.250000000000000000, -26.78125000068279604, 0.000000000000000000 ) ) ;
#9093 = CARTESIAN_POINT ( 'NONE',  ( 1.142306659890740623E-15, -30.04687499965860198, 6.218427825808274356 ) ) ;
#9094 = ORIENTED_EDGE ( 'NONE', *, *, #7383, .F. ) ;
#9095 = CARTESIAN_POINT ( 'NONE',  ( 5.385316468750001029, -29.47395833299193413, 3.109213912904134958 ) ) ;
#9096 = CARTESIAN_POINT ( 'NONE',  ( -3.492485675378566246, -6.250659073900641793, 1.467888652718973397 ) ) ;
#9097 = CARTESIAN_POINT ( 'NONE',  ( 2.033577675846918216E-14, -27.06250000000000355, 5.250000000000000888 ) ) ;
#9098 = EDGE_CURVE ( 'NONE', #5221, #7067, #7993, .T. ) ;
#9099 = CARTESIAN_POINT ( 'NONE',  ( 7.654042494670957606E-16, 69.99999999999998579, -6.250000000000000000 ) ) ;
#9100 = DIRECTION ( 'NONE',  ( 0.000000000000000000, 0.000000000000000000, -1.000000000000000000 ) ) ;
#9101 = CARTESIAN_POINT ( 'NONE',  ( 1.406733260263394847, -27.32366454968463287, -5.250000000000000000 ) ) ;
#9102 = AXIS2_PLACEMENT_3D ( 'NONE', #9171, #4936, #4294 ) ;
#9103 = CARTESIAN_POINT ( 'NONE',  ( -2.557341765625002594, -29.19270833367473017, 4.429445870380399164 ) ) ;
#9104 = CARTESIAN_POINT ( 'NONE',  ( 2.624999999999998668, -28.27083333265053255, -4.546633369868303021 ) ) ;
#9105 = PRODUCT_DEFINITION ( 'UNKNOWN', '', #1755, #3017 ) ;
#9106 = CARTESIAN_POINT ( 'NONE',  ( 5.250000000000000000, -27.81249999931720396, -6.429395695523604153E-16 ) ) ;
#9107 = CARTESIAN_POINT ( 'NONE',  ( -0.01814118441320841310, -0.6493409260993614485, 3.000000000000000444 ) ) ;
#9108 = CARTESIAN_POINT ( 'NONE',  ( 1.975475456537005874E-15, -29.43750000000000000, 5.250000000000000000 ) ) ;
#9109 = VECTOR ( 'NONE', #269, 1000.000000000000000 ) ;
#9110 = CARTESIAN_POINT ( 'NONE',  ( -5.385316468750000141, -29.32812499965859843, 0.000000000000000000 ) ) ;
#9111 = CARTESIAN_POINT ( 'NONE',  ( 4.007514324621432422, -3.650659073900639040, 1.638713065079246078 ) ) ;
#9112 = AXIS2_PLACEMENT_3D ( 'NONE', #6758, #2675, #1227 ) ;
#9113 = LINE ( 'NONE', #7591, #5395 ) ;
#9114 = CARTESIAN_POINT ( 'NONE',  ( 0.000000000000000000, -9.999999999999998224, 5.750000000000000000 ) ) ;
#9115 = CARTESIAN_POINT ( 'NONE',  ( 6.429395695523604153E-16, -27.00000000000000000, 5.250000000000000000 ) ) ;
#9116 = VECTOR ( 'NONE', #7780, 1000.000000000000000 ) ;
#9117 = EDGE_LOOP ( 'NONE', ( #1246, #2959 ) ) ;
#9118 = CARTESIAN_POINT ( 'NONE',  ( 5.250000000000000000, -29.60416666666666785, -3.031088913245536531 ) ) ;
#9119 = CARTESIAN_POINT ( 'NONE',  ( 5.114683531250000748, -27.08854166700806232, -2.952963913586932776 ) ) ;
#9120 = CARTESIAN_POINT ( 'NONE',  ( -0.01814118441314477650, -2.550659073900638951, -3.000000000000000444 ) ) ;
#9121 = CARTESIAN_POINT ( 'NONE',  ( -5.114683531249999859, -27.81770833367473017, -2.952963913586935440 ) ) ;
#9122 = DIRECTION ( 'NONE',  ( 0.000000000000000000, -1.000000000000000000, 0.000000000000000000 ) ) ;
#9123 = CARTESIAN_POINT ( 'NONE',  ( 3.616337804771879580E-16, -29.10937500034139802, -5.905927827173866440 ) ) ;
#9124 = DIRECTION ( 'NONE',  ( 0.000000000000000000, 0.000000000000000000, -1.000000000000000000 ) ) ;
#9125 = EDGE_CURVE ( 'NONE', #7425, #1822, #2977, .T. ) ;
#9126 = CARTESIAN_POINT ( 'NONE',  ( 5.114683531249998971, -29.44270833367473372, 2.952963913586936329 ) ) ;
#9127 = CARTESIAN_POINT ( 'NONE',  ( -1.000000000000000000, -35.00000000000000000, -2.880243826144208708 ) ) ;
#9128 = CARTESIAN_POINT ( 'NONE',  ( -2.624999999999996891, -29.64583333265053611, 4.546633369868304797 ) ) ;
#9129 = DIRECTION ( 'NONE',  ( 0.000000000000000000, -1.000000000000000000, 0.000000000000000000 ) ) ;
#9130 = CARTESIAN_POINT ( 'NONE',  ( -1.975475456537005874E-15, -29.59375000068279249, 5.250000000000000000 ) ) ;
#9131 = CARTESIAN_POINT ( 'NONE',  ( -5.317658234375000070, -30.03906249982930277, 0.000000000000000000 ) ) ;
#9132 = CARTESIAN_POINT ( 'NONE',  ( 2.462045979635577364, -4.049340926099360694, 2.487701488670255312 ) ) ;
#9133 = CARTESIAN_POINT ( 'NONE',  ( -3.500000000000000000, -8.249340926099360871, -0.01814118441321344033 ) ) ;
#9134 = APPLICATION_CONTEXT ( 'automotive_design' ) ;
#9135 = ORIENTED_EDGE ( 'NONE', *, *, #74, .T. ) ;
#9136 = CARTESIAN_POINT ( 'NONE',  ( 5.249999999999999112, -29.10416666666666785, -3.031088913245536975 ) ) ;
#9137 = CARTESIAN_POINT ( 'NONE',  ( -5.250000000000000000, -26.90625000068279604, -6.429395695523604153E-16 ) ) ;
#9138 = ORIENTED_EDGE ( 'NONE', *, *, #2917, .F. ) ;
#9139 = CARTESIAN_POINT ( 'NONE',  ( -2.692658234374996518, -29.28645833299193413, 4.663820869356208654 ) ) ;
#9140 = ADVANCED_FACE ( 'NONE', ( #8258 ), #7605, .F. ) ;
#9141 = CARTESIAN_POINT ( 'NONE',  ( -1.638713065079245634, -0.05065907390063852794, 4.007514324621432422 ) ) ;
#9142 = CYLINDRICAL_SURFACE ( 'NONE', #2677, 4.000000000000000000 ) ;
#9143 = CARTESIAN_POINT ( 'NONE',  ( 1.000000000000000000, -35.00000000000000000, -3.048902179152658931 ) ) ;
#9144 = CARTESIAN_POINT ( 'NONE',  ( 5.250000000000000000, -26.78125000068279604, 0.000000000000000000 ) ) ;
#9145 = DIRECTION ( 'NONE',  ( -0.000000000000000000, -0.000000000000000000, 1.000000000000000000 ) ) ;
#9146 = CARTESIAN_POINT ( 'NONE',  ( -2.557341765624999042, -28.27604166700806587, -4.429445870380400052 ) ) ;
#9147 = DIRECTION ( 'NONE',  ( 0.000000000000000000, -1.000000000000000000, 0.000000000000000000 ) ) ;
#9148 = CARTESIAN_POINT ( 'NONE',  ( -1.406733260263395735, -28.85491455036742892, 5.250000000000000000 ) ) ;
#9149 = CARTESIAN_POINT ( 'NONE',  ( -0.01814118441320841310, -7.049340926099361582, 3.000000000000000444 ) ) ;
#9150 = LINE ( 'NONE', #4270, #3697 ) ;
#9151 = CARTESIAN_POINT ( 'NONE',  ( -5.385316468750000141, -27.10937499965860198, 0.000000000000000000 ) ) ;
#9152 = CARTESIAN_POINT ( 'NONE',  ( 4.007514324621432422, -2.050659073900638507, 1.638713065079246078 ) ) ;
#9153 = CARTESIAN_POINT ( 'NONE',  ( 0.000000000000000000, -30.00000000000000000, 5.250000000000000000 ) ) ;
#9154 = ORIENTED_EDGE ( 'NONE', *, *, #7430, .F. ) ;
#9155 =( NAMED_UNIT ( * ) PLANE_ANGLE_UNIT ( ) SI_UNIT ( $, .RADIAN. ) );
#9156 = CARTESIAN_POINT ( 'NONE',  ( -5.385316468750001029, -27.34895833299193768, -3.109213912904136734 ) ) ;
#9157 = ORIENTED_EDGE ( 'NONE', *, *, #6457, .T. ) ;
#9158 = CARTESIAN_POINT ( 'NONE',  ( -1.084901341431563726E-15, -27.92187500034139802, 5.905927827173866440 ) ) ;
#9159 = CARTESIAN_POINT ( 'NONE',  ( -3.007514324621435531, -1.250659073900639573, -1.224499502706142273 ) ) ;
#9160 = CARTESIAN_POINT ( 'NONE',  ( 5.250000000000000000, -29.47916666666666430, -3.031088913245534755 ) ) ;
#9161 = DIRECTION ( 'NONE',  ( 0.000000000000000000, 0.000000000000000000, 1.000000000000000000 ) ) ;
#9162 = STYLED_ITEM ( 'NONE', ( #4382 ), #417 ) ;
#9163 = EDGE_CURVE ( 'NONE', #8139, #3879, #7276, .T. ) ;
#9164 = CARTESIAN_POINT ( 'NONE',  ( 5.114683531250000748, -29.65104166700806232, -2.952963913586932776 ) ) ;
#9165 = CARTESIAN_POINT ( 'NONE',  ( -1.084901341431563923E-15, -27.73437500034139802, 5.905927827173866440 ) ) ;
#9166 = CARTESIAN_POINT ( 'NONE',  ( -5.249999999999999112, -29.27083333333333570, -3.031088913245534755 ) ) ;
#9167 = CARTESIAN_POINT ( 'NONE',  ( -2.625000000000000444, -29.72916666598387181, -4.546633369868303021 ) ) ;
#9168 = CARTESIAN_POINT ( 'NONE',  ( 1.406733260263395735, -27.61383544963257108, 5.250000000000000000 ) ) ;
#9169 = EDGE_CURVE ( 'NONE', #8745, #2693, #5590, .T. ) ;
#9170 =( NAMED_UNIT ( * ) SI_UNIT ( $, .STERADIAN. ) SOLID_ANGLE_UNIT ( ) );
#9171 = CARTESIAN_POINT ( 'NONE',  ( 0.000000000000000000, -27.00000000000000000, 0.000000000000000000 ) ) ;
#9172 = CARTESIAN_POINT ( 'NONE',  ( 1.467888652719048226, -1.349340926099361182, -3.492485675378536047 ) ) ;
#9173 = CARTESIAN_POINT ( 'NONE',  ( -1.431606283892620235, -7.949340926099361049, -3.507514324621463953 ) ) ;
#9174 = ORIENTED_EDGE ( 'NONE', *, *, #4012, .T. ) ;
#9175 = CARTESIAN_POINT ( 'NONE',  ( 1.406733260263393293, -29.07366454968462577, -5.250000000000000000 ) ) ;
#9176 = CARTESIAN_POINT ( 'NONE',  ( -5.114683531250000748, -29.73437500034139802, -6.263680815196995234E-16 ) ) ;
#9177 = EDGE_LOOP ( 'NONE', ( #631, #2281 ) ) ;
#9178 = CARTESIAN_POINT ( 'NONE',  ( 5.385316468750000141, -29.95312499965859843, -6.595110575850215044E-16 ) ) ;
#9179 = CARTESIAN_POINT ( 'NONE',  ( -0.01814118441313947866, -7.350659073900638774, -3.500000000000000000 ) ) ;
#9180 = CARTESIAN_POINT ( 'NONE',  ( 6.429395695523604153E-16, -27.00000000000000000, 5.250000000000000000 ) ) ;
#9181 = CIRCLE ( 'NONE', #575, 4.250000000000000000 ) ;
#9182 = ORIENTED_EDGE ( 'NONE', *, *, #7525, .T. ) ;
#9183 = LINE ( 'NONE', #4908, #7893 ) ;
#9184 = CARTESIAN_POINT ( 'NONE',  ( 0.000000000000000000, -27.00000000000000000, 0.000000000000000000 ) ) ;
#9185 = CARTESIAN_POINT ( 'NONE',  ( 5.250000000000000000, -27.31249999931720396, -6.429395695523604153E-16 ) ) ;
#9186 = AXIS2_PLACEMENT_3D ( 'NONE', #356, #3208, #1289 ) ;
#9187 = CARTESIAN_POINT ( 'NONE',  ( -1.084901341431563923E-15, -28.92187500034139447, 5.905927827173866440 ) ) ;
#9188 = CIRCLE ( 'NONE', #7583, 4.000000000000000000 ) ;
#9189 = NEXT_ASSEMBLY_USAGE_OCCURRENCE ( 'NAUO1', ' ', ' ', #741, #3486, $ ) ;
#9190 = NEXT_ASSEMBLY_USAGE_OCCURRENCE ( 'NAUO2', ' ', ' ', #741, #5115, $ ) ;
#9191 = NEXT_ASSEMBLY_USAGE_OCCURRENCE ( 'NAUO3', ' ', ' ', #741, #9105, $ ) ;
#9192 = NEXT_ASSEMBLY_USAGE_OCCURRENCE ( 'NAUO4', ' ', ' ', #741, #4331, $ ) ;
#9193 = NEXT_ASSEMBLY_USAGE_OCCURRENCE ( 'NAUO5', ' ', ' ', #741, #1543, $ ) ;
#9194 = NEXT_ASSEMBLY_USAGE_OCCURRENCE ( 'NAUO6', ' ', ' ', #741, #3942, $ ) ;
#9195 = NEXT_ASSEMBLY_USAGE_OCCURRENCE ( 'NAUO7', ' ', ' ', #741, #6653, $ ) ;
#9196 = NEXT_ASSEMBLY_USAGE_OCCURRENCE ( 'NAUO8', ' ', ' ', #741, #8320, $ ) ;
#9197 = NEXT_ASSEMBLY_USAGE_OCCURRENCE ( 'NAUO9', ' ', ' ', #741, #349, $ ) ;
#9198=COLOUR_RGB('Dark Blue',0.08,0.2,0.34);
#9199=FILL_AREA_STYLE_COLOUR('',#9198);
#9200=FILL_AREA_STYLE('',(#9199));
#9201=SURFACE_STYLE_FILL_AREA(#9200);
#9202=SURFACE_SIDE_STYLE('',(#9201));
#9203=SURFACE_STYLE_USAGE(.BOTH.,#9202);
#9204=PRESENTATION_STYLE_ASSIGNMENT((#9203));
#9205=COLOUR_RGB('Light Blue',0.38,0.62,0.78);
#9206=FILL_AREA_STYLE_COLOUR('',#9205);
#9207=FILL_AREA_STYLE('',(#9206));
#9208=SURFACE_STYLE_FILL_AREA(#9207);
#9209=SURFACE_SIDE_STYLE('',(#9208));
#9210=SURFACE_STYLE_USAGE(.BOTH.,#9209);
#9211=PRESENTATION_STYLE_ASSIGNMENT((#9210));
#9212=COLOUR_RGB('Sky Blue',0.24,0.69,0.87);
#9213=FILL_AREA_STYLE_COLOUR('',#9212);
#9214=FILL_AREA_STYLE('',(#9213));
#9215=SURFACE_STYLE_FILL_AREA(#9214);
#9216=SURFACE_SIDE_STYLE('',(#9215));
#9217=SURFACE_STYLE_USAGE(.BOTH.,#9216);
#9218=PRESENTATION_STYLE_ASSIGNMENT((#9217));
#9219=COLOUR_RGB('Grey',0.48,0.52,0.57);
#9220=FILL_AREA_STYLE_COLOUR('',#9219);
#9221=FILL_AREA_STYLE('',(#9220));
#9222=SURFACE_STYLE_FILL_AREA(#9221);
#9223=SURFACE_SIDE_STYLE('',(#9222));
#9224=SURFACE_STYLE_USAGE(.BOTH.,#9223);
#9225=PRESENTATION_STYLE_ASSIGNMENT((#9224));
#9226=COLOUR_RGB('Black',0.12,0.14,0.17);
#9227=FILL_AREA_STYLE_COLOUR('',#9226);
#9228=FILL_AREA_STYLE('',(#9227));
#9229=SURFACE_STYLE_FILL_AREA(#9228);
#9230=SURFACE_SIDE_STYLE('',(#9229));
#9231=SURFACE_STYLE_USAGE(.BOTH.,#9230);
#9232=PRESENTATION_STYLE_ASSIGNMENT((#9231));
#9233=COLOUR_RGB('Off White',0.89,0.88,0.83);
#9234=FILL_AREA_STYLE_COLOUR('',#9233);
#9235=FILL_AREA_STYLE('',(#9234));
#9236=SURFACE_STYLE_FILL_AREA(#9235);
#9237=SURFACE_SIDE_STYLE('',(#9236));
#9238=SURFACE_STYLE_USAGE(.BOTH.,#9237);
#9239=PRESENTATION_STYLE_ASSIGNMENT((#9238));
ENDSEC;
END-ISO-10303-21;
